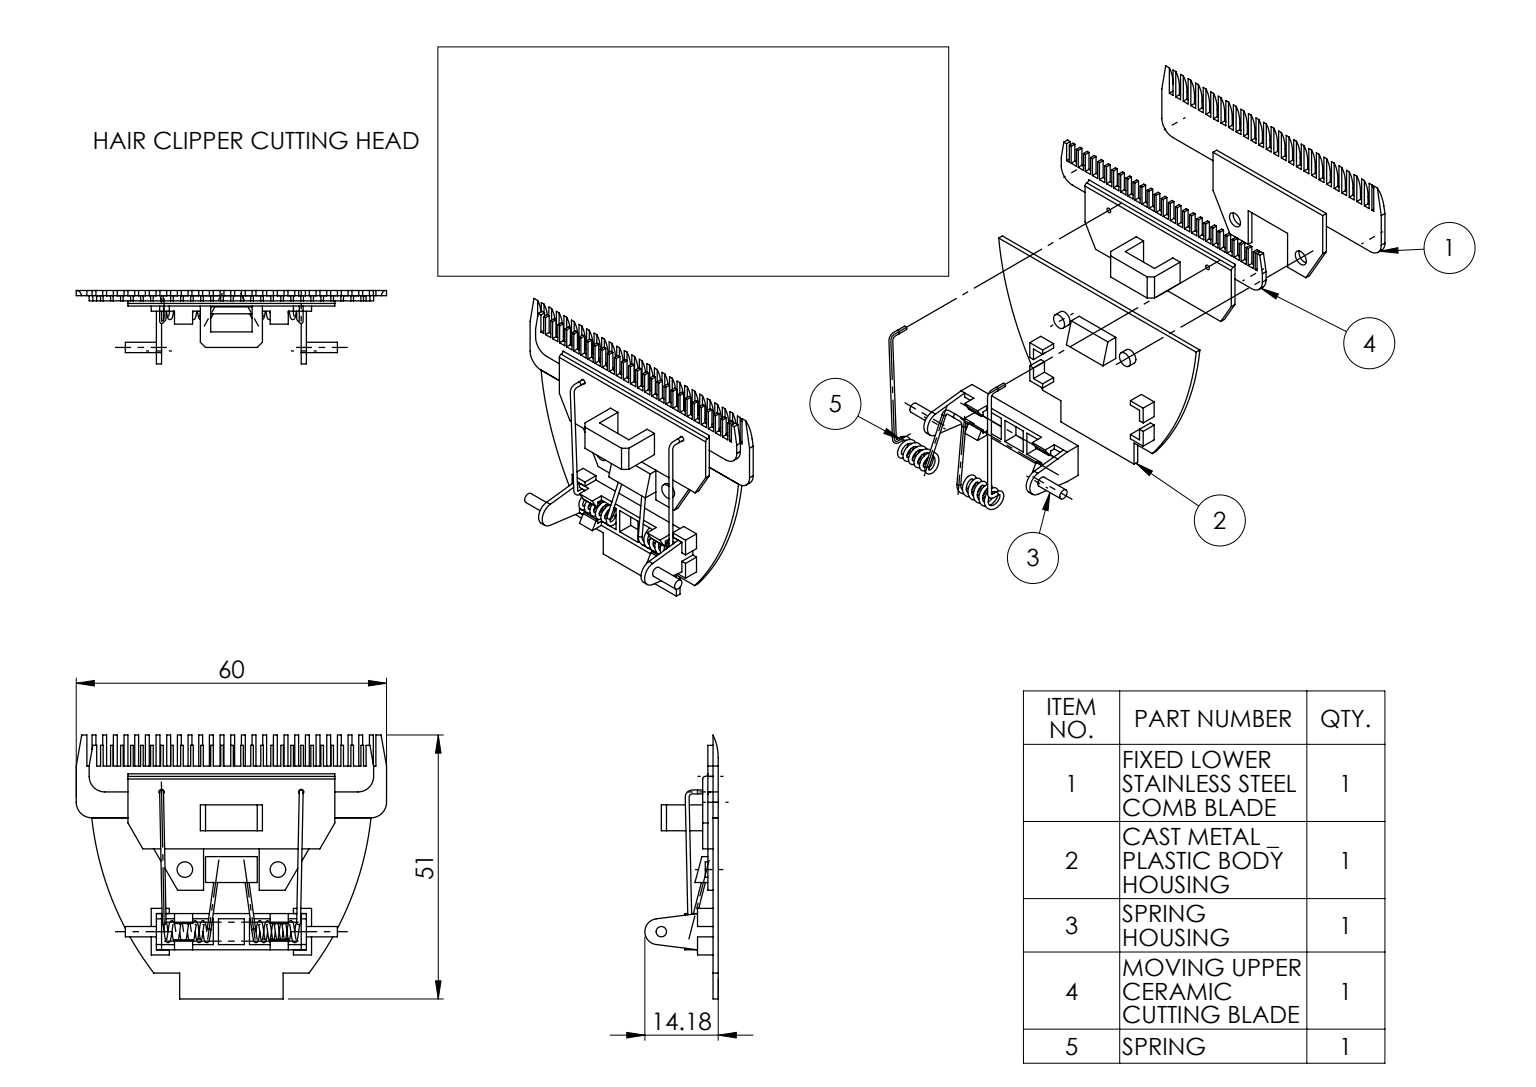
ISO-10303-21;
HEADER;
FILE_DESCRIPTION (('STEP AP214'),
    '1' );
FILE_NAME ('BR-832',
    '2026-10-04T16:38:04',
    ( '' ),
    ( '' ),
    'SwSTEP 2.0',
    'SolidWorks 2026',
    '' );
FILE_SCHEMA (( 'AUTOMOTIVE_DESIGN' ));
ENDSEC;

DATA;
#1 = EDGE_CURVE ( 'NONE', #8973, #13899, #6324, .T. ) ;
#2 = DIRECTION ( 'NONE',  ( -1.000000000000000000, 0.000000000000000000, 0.000000000000000000 ) ) ;
#3 = CARTESIAN_POINT ( 'NONE',  ( -13.45643611822145225, -15.38747602984844853, 4.825999963382285429 ) ) ;
#4 = CARTESIAN_POINT ( 'NONE',  ( 8.871558582316794173, -20.24999999999999289, 3.449312527122348371 ) ) ;
#5 = CARTESIAN_POINT ( 'NONE',  ( -12.62499963760179256, -21.00001830110826972, 4.442557003548452066 ) ) ;
#6 = AXIS2_PLACEMENT_3D ( 'NONE', #19220, #15754, #1437 ) ;
#7 = VECTOR ( 'NONE', #16168, 1000.000000000000000 ) ;
#8 = CARTESIAN_POINT ( 'NONE',  ( -22.81633994409548549, 11.64110105645932691, 0.000000000000000000 ) ) ;
#9 = CARTESIAN_POINT ( 'NONE',  ( -8.309058582316795949, -23.80360840875935935, 1.768074502826626260 ) ) ;
#10 = CARTESIAN_POINT ( 'NONE',  ( 8.496558582316794173, -22.05068747287764452, 1.749999999999998446 ) ) ;
#11 = CARTESIAN_POINT ( 'NONE',  ( 4.097191417683177406, -22.46490103525075810, 4.479004561291653808 ) ) ;
#12 = CARTESIAN_POINT ( 'NONE',  ( -6.621558582316794173, -23.74999999999999645, 3.550687472877651629 ) ) ;
#13 = VERTEX_POINT ( 'NONE', #12698 ) ;
#14 = CARTESIAN_POINT ( 'NONE',  ( 13.82092246150448211, 3.019084305971233562, 5.221833296715730377 ) ) ;
#15 = VECTOR ( 'NONE', #20550, 1000.000000000000000 ) ;
#16 = CARTESIAN_POINT ( 'NONE',  ( -13.49999999999998401, -21.99999999999999645, 11.68378559369222280 ) ) ;
#17 = VERTEX_POINT ( 'NONE', #19101 ) ;
#18 = AXIS2_PLACEMENT_3D ( 'NONE', #8053, #6581, #4805 ) ;
#19 = VERTEX_POINT ( 'NONE', #1418 ) ;
#20 = CARTESIAN_POINT ( 'NONE',  ( 29.44326362367961636, 13.15740888934567288, -2.785412301099487325E-16 ) ) ;
#21 = FACE_BOUND ( 'NONE', #10951, .T. ) ;
#22 = VECTOR ( 'NONE', #3512, 1000.000000000000000 ) ;
#23 = CIRCLE ( 'NONE', #12706, 10.00000000000000000 ) ;
#24 = DIRECTION ( 'NONE',  ( 1.000000000000000000, 0.000000000000000000, 0.000000000000000000 ) ) ;
#25 = CARTESIAN_POINT ( 'NONE',  ( -1.548630333695928396, -9.114917468222230923, 2.372643865078341019 ) ) ;
#26 = FACE_OUTER_BOUND ( 'NONE', #4692, .T. ) ;
#27 = EDGE_CURVE ( 'NONE', #6657, #12771, #12900, .T. ) ;
#28 = CARTESIAN_POINT ( 'NONE',  ( 2.506848361495492394, -9.459347215042898327, 1.711100304737409150 ) ) ;
#29 = CARTESIAN_POINT ( 'NONE',  ( -13.10012427866737639, 3.743776072700027324, 6.001983176248468332 ) ) ;
#30 = CARTESIAN_POINT ( 'NONE',  ( 9.715308582316794173, -23.77099543870833998, 2.825813738724734847 ) ) ;
#31 = CARTESIAN_POINT ( 'NONE',  ( -18.69064177244175795, 11.64110105645932691, 0.000000000000000000 ) ) ;
#32 = CARTESIAN_POINT ( 'NONE',  ( 13.15498530132288479, 5.764257716805535559, 4.666666666666618113 ) ) ;
#33 = CARTESIAN_POINT ( 'NONE',  ( -1.797685059409938280, -9.880079706704160358, 1.626537830816663588 ) ) ;
#34 = ADVANCED_FACE ( 'NONE', ( #11140 ), #17508, .F. ) ;
#35 = ORIENTED_EDGE ( 'NONE', *, *, #2432, .F. ) ;
#36 = ADVANCED_FACE ( 'NONE', ( #7996 ), #7800, .T. ) ;
#37 = CARTESIAN_POINT ( 'NONE',  ( -13.85980676119184629, 4.232741440188380722, 5.965367510457697975 ) ) ;
#38 = CARTESIAN_POINT ( 'NONE',  ( 0.000000000000000000, 10.00000000000000000, 1.000000000000000000 ) ) ;
#39 = CIRCLE ( 'NONE', #18741, 9.999999999999998224 ) ;
#40 = CARTESIAN_POINT ( 'NONE',  ( 5.972191417683178294, -24.47900456129165292, 2.413778621189595963 ) ) ;
#41 = CARTESIAN_POINT ( 'NONE',  ( -6.534691417683177406, -20.97900456129164581, 3.136473910504570917 ) ) ;
#42 = VERTEX_POINT ( 'NONE', #6438 ) ;
#43 = VECTOR ( 'NONE', #1167, 1000.000000000000000 ) ;
#44 = CARTESIAN_POINT ( 'NONE',  ( 13.90439735423812273, 5.734566389025032684, 4.166666666666765551 ) ) ;
#45 = CARTESIAN_POINT ( 'NONE',  ( 13.11017182064853159, 4.251176942750957366, 5.979809059808775196 ) ) ;
#46 = DIRECTION ( 'NONE',  ( 1.000000000000000000, -6.938893903907222067E-15, 0.000000000000000000 ) ) ;
#47 = VECTOR ( 'NONE', #8617, 1000.000000000000000 ) ;
#48 = EDGE_LOOP ( 'NONE', ( #6607, #18673, #6407, #16806 ) ) ;
#49 = VERTEX_POINT ( 'NONE', #11237 ) ;
#50 = PLANE ( 'NONE',  #13438 ) ;
#51 = PLANE ( 'NONE',  #17586 ) ;
#52 = DIRECTION ( 'NONE',  ( 0.000000000000000000, 0.000000000000000000, 1.000000000000000000 ) ) ;
#53 = LINE ( 'NONE', #6129, #8350 ) ;
#54 = AXIS2_PLACEMENT_3D ( 'NONE', #18555, #20450, #10501 ) ;
#55 = EDGE_CURVE ( 'NONE', #14709, #7180, #17615, .T. ) ;
#56 = LINE ( 'NONE', #9565, #7988 ) ;
#57 = CARTESIAN_POINT ( 'NONE',  ( 2.097836924194969033, -11.64739567274323129, 2.830419876579102212 ) ) ;
#58 = LINE ( 'NONE', #8001, #5190 ) ;
#59 = LINE ( 'NONE', #8216, #18452 ) ;
#60 = CARTESIAN_POINT ( 'NONE',  ( 10.05565079891005631, 0.000000000000000000, 1.000000000000000000 ) ) ;
#61 = LINE ( 'NONE', #4966, #6978 ) ;
#62 = DIRECTION ( 'NONE',  ( -5.782411586589356653E-16, 1.000000000000000000, 0.000000000000000000 ) ) ;
#63 = DIRECTION ( 'NONE',  ( 1.000000000000000000, 0.000000000000000000, 0.000000000000000000 ) ) ;
#64 = CARTESIAN_POINT ( 'NONE',  ( 11.77780858231679595, -21.02099543870833998, 3.035098964749253003 ) ) ;
#65 = CARTESIAN_POINT ( 'NONE',  ( -13.08799567112409790, 3.881281391764801025, 5.254907606674271037 ) ) ;
#66 = CARTESIAN_POINT ( 'NONE',  ( -5.309058582316795949, -22.74294823697954016, 2.828734674606448785 ) ) ;
#67 = CARTESIAN_POINT ( 'NONE',  ( -12.25344141768317741, -21.94931252712233061, 1.749999999999998446 ) ) ;
#68 = VERTEX_POINT ( 'NONE', #1726 ) ;
#69 = CARTESIAN_POINT ( 'NONE',  ( 13.09358652029869141, 4.163619275088517035, 5.207983256689002083 ) ) ;
#70 = SURFACE_STYLE_USAGE ( .BOTH. , #17121 ) ;
#71 = ORIENTED_EDGE ( 'NONE', *, *, #17925, .T. ) ;
#72 = ORIENTED_EDGE ( 'NONE', *, *, #11352, .T. ) ;
#73 = AXIS2_PLACEMENT_3D ( 'NONE', #7626, #20402, #7929 ) ;
#74 = DIRECTION ( 'NONE',  ( 1.000000000000000000, 0.000000000000000000, -0.000000000000000000 ) ) ;
#75 = CARTESIAN_POINT ( 'NONE',  ( 13.37505392270939986, -20.99727690317663686, 4.612442573673130930 ) ) ;
#76 = ORIENTED_EDGE ( 'NONE', *, *, #12428, .T. ) ;
#77 = LINE ( 'NONE', #272, #14093 ) ;
#78 = ORIENTED_EDGE ( 'NONE', *, *, #4872, .F. ) ;
#79 = CARTESIAN_POINT ( 'NONE',  ( 10.19094141768317563, -23.27327832286946219, 4.701595411283453707 ) ) ;
#80 = DIRECTION ( 'NONE',  ( -0.000000000000000000, -0.000000000000000000, -1.000000000000000000 ) ) ;
#81 = EDGE_CURVE ( 'NONE', #12312, #20463, #4960, .T. ) ;
#82 = EDGE_CURVE ( 'NONE', #4544, #2802, #3495, .T. ) ;
#83 = CARTESIAN_POINT ( 'NONE',  ( -2.583953725994688533, -9.847075946378776479, 2.560676788604062004 ) ) ;
#84 = CARTESIAN_POINT ( 'NONE',  ( 2.702705060698113115, -10.69015907548275379, 2.777197378435510622 ) ) ;
#85 = CARTESIAN_POINT ( 'NONE',  ( -10.65280858231679240, -21.22443879296942626, 5.229004561291660025 ) ) ;
#86 = VECTOR ( 'NONE', #19310, 1000.000000000000114 ) ;
#87 = LINE ( 'NONE', #11371, #8961 ) ;
#88 = CARTESIAN_POINT ( 'NONE',  ( 5.503441417683177406, -22.05068747287766229, 6.000000000000001776 ) ) ;
#89 =( NAMED_UNIT ( * ) PLANE_ANGLE_UNIT ( ) SI_UNIT ( $, .RADIAN. ) );
#90 = CARTESIAN_POINT ( 'NONE',  ( -3.974842109207561425, -21.82955800590261575, 5.256404853634145447 ) ) ;
#91 = ORIENTED_EDGE ( 'NONE', *, *, #1253, .F. ) ;
#92 = CARTESIAN_POINT ( 'NONE',  ( 13.37155858231679595, -19.49999999999998934, 3.449312527122348371 ) ) ;
#93 = DIRECTION ( 'NONE',  ( -0.000000000000000000, -0.000000000000000000, -1.000000000000000000 ) ) ;
#94 = CARTESIAN_POINT ( 'NONE',  ( -13.90439735423812273, 5.734566389025032684, 4.791666666666684726 ) ) ;
#95 = VERTEX_POINT ( 'NONE', #2332 ) ;
#96 = ADVANCED_FACE ( 'NONE', ( #6747 ), #14788, .T. ) ;
#97 = CARTESIAN_POINT ( 'NONE',  ( 7.465308582316795061, -20.22900456129164937, 4.174186261275266929 ) ) ;
#98 = DIRECTION ( 'NONE',  ( 0.000000000000000000, 1.000000000000000000, 0.000000000000000000 ) ) ;
#99 = ORIENTED_EDGE ( 'NONE', *, *, #2749, .T. ) ;
#100 = DIRECTION ( 'NONE',  ( 0.000000000000000000, 1.000000000000000000, 0.000000000000000000 ) ) ;
#101 = EDGE_LOOP ( 'NONE', ( #4164, #18704, #19121, #9760 ) ) ;
#102 = VECTOR ( 'NONE', #3699, 1000.000000000000000 ) ;
#103 = LINE ( 'NONE', #17562, #12127 ) ;
#104 = ORIENTED_EDGE ( 'NONE', *, *, #13146, .F. ) ;
#105 = CARTESIAN_POINT ( 'NONE',  ( -12.43405858231679595, -23.73192549717337130, 5.303608408759367343 ) ) ;
#106 = CARTESIAN_POINT ( 'NONE',  ( 12.62499979224180180, -20.25001049178813162, 4.458178821399696012 ) ) ;
#107 = DIRECTION ( 'NONE',  ( -1.000000000000000000, 0.000000000000000000, 0.000000000000000000 ) ) ;
#108 = CARTESIAN_POINT ( 'NONE',  ( 0.5631383031621635116, -9.114917468222230923, 1.622643865078341463 ) ) ;
#109 = CARTESIAN_POINT ( 'NONE',  ( 12.62499999999998579, -20.24999999999999289, 3.666666666666653640 ) ) ;
#110 = CARTESIAN_POINT ( 'NONE',  ( -11.00000000000000000, -25.49999999999999645, 6.500000000000000000 ) ) ;
#111 = CARTESIAN_POINT ( 'NONE',  ( -13.37499999999998579, -20.24999999999999289, 3.146526952850934755 ) ) ;
#112 = CARTESIAN_POINT ( 'NONE',  ( 7.840308582316794173, -22.67418626127525982, 5.270995438708342640 ) ) ;
#113 = CARTESIAN_POINT ( 'NONE',  ( -13.89992416064626646, 5.508670112635706495, 5.888743936161951353 ) ) ;
#114 = VECTOR ( 'NONE', #15578, 1000.000000000000000 ) ;
#115 = LINE ( 'NONE', #12457, #8728 ) ;
#116 = CARTESIAN_POINT ( 'NONE',  ( -10.74655858231679595, -21.94931252712234127, 6.000000000000001776 ) ) ;
#117 = CARTESIAN_POINT ( 'NONE',  ( 4.840308582316793284, -22.67418626127525982, 5.270995438708342640 ) ) ;
#118 = EDGE_CURVE ( 'NONE', #8944, #9004, #361, .T. ) ;
#119 = CARTESIAN_POINT ( 'NONE',  ( 8.503441417683177406, -22.05068747287766229, 4.499999999999999112 ) ) ;
#120 = CARTESIAN_POINT ( 'NONE',  ( -9.815941417683177406, -20.79840458871654363, 4.773278322869464851 ) ) ;
#121 = ORIENTED_EDGE ( 'NONE', *, *, #545, .F. ) ;
#122 = VERTEX_POINT ( 'NONE', #13311 ) ;
#123 = CARTESIAN_POINT ( 'NONE',  ( 13.80173896975277437, 2.050317972508536535, 5.200999963382010094 ) ) ;
#124 = CARTESIAN_POINT ( 'NONE',  ( 27.94203811574920948, 16.00000000000000000, 1.000000000000000000 ) ) ;
#125 = CARTESIAN_POINT ( 'NONE',  ( 2.693754455098655409, -10.04853567022903782, 2.237415670251142519 ) ) ;
#126 = ORIENTED_EDGE ( 'NONE', *, *, #7427, .F. ) ;
#127 = EDGE_LOOP ( 'NONE', ( #2197, #15477, #13303, #7881 ) ) ;
#128 = CARTESIAN_POINT ( 'NONE',  ( 5.683390479346035029, 0.000000000000000000, 0.000000000000000000 ) ) ;
#129 = CARTESIAN_POINT ( 'NONE',  ( 0.000000000000000000, 11.64110105645932691, 10.00000000000000000 ) ) ;
#130 = FACE_OUTER_BOUND ( 'NONE', #18306, .T. ) ;
#131 = APPLICATION_CONTEXT ( 'automotive_design' ) ;
#132 = CARTESIAN_POINT ( 'NONE',  ( -2.076833265075072266, -8.407161531158021006, 2.383492984350220389 ) ) ;
#133 = CARTESIAN_POINT ( 'NONE',  ( 0.2815691515810352930, -9.114917468222230923, 2.372643865078523984 ) ) ;
#134 = CARTESIAN_POINT ( 'NONE',  ( -15.11404127825609223, 9.000000000000001776, 0.000000000000000000 ) ) ;
#135 = CARTESIAN_POINT ( 'NONE',  ( -13.09532840572934376, 3.501584489333809724, 5.996774842915142401 ) ) ;
#136 = DIRECTION ( 'NONE',  ( 0.000000000000000000, 0.000000000000000000, -1.000000000000000000 ) ) ;
#137 = LINE ( 'NONE', #12477, #19758 ) ;
#138 = CARTESIAN_POINT ( 'NONE',  ( 13.12175473207386922, 4.086113969730903683, 6.756475741440692850 ) ) ;
#139 = CARTESIAN_POINT ( 'NONE',  ( -1.982945319006538032, -10.83166796549307520, 2.620924705558935308 ) ) ;
#140 = ORIENTED_EDGE ( 'NONE', *, *, #2638, .T. ) ;
#141 = CARTESIAN_POINT ( 'NONE',  ( -13.37499999998404299, -20.99999999996810729, 2.793053905886972998 ) ) ;
#142 = CARTESIAN_POINT ( 'NONE',  ( 6.063547257480584207, 10.00000000000000000, 1.000000000000000000 ) ) ;
#143 = CARTESIAN_POINT ( 'NONE',  ( 5.878441417683177406, -24.50000000000000000, 3.449312527122335048 ) ) ;
#144 = CARTESIAN_POINT ( 'NONE',  ( -6.809058582316796837, -22.74294823697954016, 2.828734674606448785 ) ) ;
#145 = EDGE_LOOP ( 'NONE', ( #572, #13357 ) ) ;
#146 = CARTESIAN_POINT ( 'NONE',  ( 12.62608183053121458, -20.94536755816881168, 4.949360998036265613 ) ) ;
#147 = CARTESIAN_POINT ( 'NONE',  ( 13.10557919622060652, 4.019249409169220577, 6.007898877577752650 ) ) ;
#148 = CARTESIAN_POINT ( 'NONE',  ( -24.79469207716615031, 9.000000000000001776, 1.000000000000000000 ) ) ;
#149 = EDGE_LOOP ( 'NONE', ( #17432, #19814, #17504, #3948 ) ) ;
#150 = EDGE_CURVE ( 'NONE', #20096, #3927, #16331, .T. ) ;
#151 = ORIENTED_EDGE ( 'NONE', *, *, #14900, .F. ) ;
#152 = CARTESIAN_POINT ( 'NONE',  ( -27.94203811574921659, 9.999999999999998224, 1.000000000000000000 ) ) ;
#153 = DIRECTION ( 'NONE',  ( 1.734723475976807094E-15, -1.000000000000000000, 0.000000000000000000 ) ) ;
#154 = EDGE_CURVE ( 'NONE', #3175, #3359, #11545, .T. ) ;
#155 = EDGE_CURVE ( 'NONE', #9432, #10023, #14985, .T. ) ;
#156 = ORIENTED_EDGE ( 'NONE', *, *, #12533, .T. ) ;
#157 = CARTESIAN_POINT ( 'NONE',  ( 0.000000000000000000, 10.00000000000000000, 1.000000000000000000 ) ) ;
#158 = CARTESIAN_POINT ( 'NONE',  ( 0.2815691515810352374, -9.864917468222230923, 1.622643865078524428 ) ) ;
#159 = DIRECTION ( 'NONE',  ( 1.000000000000000000, 0.000000000000000000, 0.000000000000000000 ) ) ;
#160 = CARTESIAN_POINT ( 'NONE',  ( 27.00000000000000000, 3.000000000000000000, 1.000000000000000000 ) ) ;
#161 = CARTESIAN_POINT ( 'NONE',  ( 0.3749999999999968914, 9.000000000000000000, 1.000000000000000000 ) ) ;
#162 = DIRECTION ( 'NONE',  ( -0.000000000000000000, -0.000000000000000000, -1.000000000000000000 ) ) ;
#163 = CARTESIAN_POINT ( 'NONE',  ( -11.12155858231679417, -23.74999999999999645, 3.550687472877651629 ) ) ;
#164 = CARTESIAN_POINT ( 'NONE',  ( -13.09734501894798342, -20.62502179913553846, 3.486720336327766567 ) ) ;
#165 = CARTESIAN_POINT ( 'NONE',  ( -13.08559773465513487, 3.760185600081874746, 5.252303440007609403 ) ) ;
#166 = CARTESIAN_POINT ( 'NONE',  ( -10.84030858231679240, -22.67418626127525982, 5.270995438708342640 ) ) ;
#167 = CARTESIAN_POINT ( 'NONE',  ( -8.784691417683177406, -23.77099543870834353, 4.174186261275252718 ) ) ;
#168 = EDGE_LOOP ( 'NONE', ( #6512, #8849, #9507, #11718, #13942, #16405 ) ) ;
#169 = CARTESIAN_POINT ( 'NONE',  ( 13.37893135632597819, -19.30146650553847465, 4.738802066438188909 ) ) ;
#170 = DIRECTION ( 'NONE',  ( -0.000000000000000000, -0.000000000000000000, -1.000000000000000000 ) ) ;
#171 = ORIENTED_EDGE ( 'NONE', *, *, #6216, .T. ) ;
#172 = ORIENTED_EDGE ( 'NONE', *, *, #1116, .F. ) ;
#173 = DIRECTION ( 'NONE',  ( -0.000000000000000000, -0.000000000000000000, -1.000000000000000000 ) ) ;
#174 = EDGE_CURVE ( 'NONE', #8535, #2052, #465, .T. ) ;
#175 = VERTEX_POINT ( 'NONE', #3806 ) ;
#176 = CARTESIAN_POINT ( 'NONE',  ( -15.00000000000000000, 3.000000000000000000, 1.000000000000000000 ) ) ;
#177 = ORIENTED_EDGE ( 'NONE', *, *, #14375, .F. ) ;
#178 = CARTESIAN_POINT ( 'NONE',  ( 9.628441417683177406, -20.24999999999999289, 3.550687472877664952 ) ) ;
#179 = FACE_OUTER_BOUND ( 'NONE', #19675, .T. ) ;
#180 = AXIS2_PLACEMENT_3D ( 'NONE', #10679, #7642, #12344 ) ;
#181 = CARTESIAN_POINT ( 'NONE',  ( -1.710927537542899612, -9.866086492083725901, 2.372944093759576933 ) ) ;
#182 = CARTESIAN_POINT ( 'NONE',  ( 2.659620708751979645, -10.38426118526329489, 2.698636689302993830 ) ) ;
#183 = CARTESIAN_POINT ( 'NONE',  ( -11.87155858231679417, -20.24999999999999289, 3.449312527122348371 ) ) ;
#184 = EDGE_CURVE ( 'NONE', #2924, #1770, #13210, .T. ) ;
#185 = FILL_AREA_STYLE ('',( #1857 ) ) ;
#186 = CARTESIAN_POINT ( 'NONE',  ( 7.190941417683176518, -23.27327832286946219, 4.701595411283453707 ) ) ;
#187 = LINE ( 'NONE', #10011, #17890 ) ;
#188 = CARTESIAN_POINT ( 'NONE',  ( -6.253441417683176518, -21.94931252712233061, 1.749999999999998446 ) ) ;
#189 = ORIENTED_EDGE ( 'NONE', *, *, #9219, .F. ) ;
#190 = CARTESIAN_POINT ( 'NONE',  ( 11.30905858231679595, -23.80360840875935935, 1.768074502826626260 ) ) ;
#191 = CARTESIAN_POINT ( 'NONE',  ( 12.64387510712649565, -19.29680709011273976, 5.506486987317513737 ) ) ;
#192 = CARTESIAN_POINT ( 'NONE',  ( -12.62562019941893432, -20.21867992933967173, 4.757612834768309540 ) ) ;
#193 = VERTEX_POINT ( 'NONE', #561 ) ;
#194 = FACE_OUTER_BOUND ( 'NONE', #14246, .T. ) ;
#195 = EDGE_CURVE ( 'NONE', #11770, #17871, #16650, .T. ) ;
#196 = LINE ( 'NONE', #13157, #16335 ) ;
#197 = EDGE_CURVE ( 'NONE', #4053, #10774, #19608, .T. ) ;
#198 = EDGE_LOOP ( 'NONE', ( #19605, #1454, #13205, #13918 ) ) ;
#199 = SHAPE_DEFINITION_REPRESENTATION ( #15847, #6045 ) ;
#200 = VERTEX_POINT ( 'NONE', #10184 ) ;
#201 = CARTESIAN_POINT ( 'NONE',  ( -8.376396343307449754, 11.64110105645932691, 0.000000000000000000 ) ) ;
#202 = ORIENTED_EDGE ( 'NONE', *, *, #15005, .F. ) ;
#203 = CARTESIAN_POINT ( 'NONE',  ( -7.277808582316794173, -20.27099543870833642, 2.724438792969431589 ) ) ;
#204 = DIRECTION ( 'NONE',  ( 0.000000000000000000, -1.000000000000000000, 0.000000000000000000 ) ) ;
#205 = DIRECTION ( 'NONE',  ( 0.000000000000000000, -1.000000000000000000, 0.000000000000000000 ) ) ;
#206 = CARTESIAN_POINT ( 'NONE',  ( 2.022757268986824730, -10.07035769906783784, 1.675405020440470238 ) ) ;
#207 = CARTESIAN_POINT ( 'NONE',  ( 12.65410809543883985, -18.78004118034163739, 5.517608176248461227 ) ) ;
#208 = DIRECTION ( 'NONE',  ( -0.9848077530122082424, 0.1736481776669295263, 0.000000000000000000 ) ) ;
#209 = CARTESIAN_POINT ( 'NONE',  ( -13.39169183355864590, -18.65706240528901105, 4.755687463382285429 ) ) ;
#210 = CARTESIAN_POINT ( 'NONE',  ( 8.777808582316797725, -19.52099543870833642, 2.413778621189609286 ) ) ;
#211 = CARTESIAN_POINT ( 'NONE',  ( -12.62500000000001954, -20.24999999999450040, 3.833333333368183382 ) ) ;
#212 = DIRECTION ( 'NONE',  ( -1.000000000000000000, -6.938893903907222067E-15, 0.000000000000000000 ) ) ;
#213 = CARTESIAN_POINT ( 'NONE',  ( 5.215308582316793284, -23.77099543870833998, 2.825813738724734847 ) ) ;
#214 = CARTESIAN_POINT ( 'NONE',  ( 4.565941417683176518, -22.67126532539353789, 2.757051763020445634 ) ) ;
#215 = CARTESIAN_POINT ( 'NONE',  ( -5.409691417683177406, -21.32581373872474373, 5.270995438708348857 ) ) ;
#216 = ORIENTED_EDGE ( 'NONE', *, *, #5288, .T. ) ;
#217 = ORIENTED_EDGE ( 'NONE', *, *, #4935, .T. ) ;
#218 = CARTESIAN_POINT ( 'NONE',  ( 13.82811627091129836, 3.382371681020614584, 5.229645796715683304 ) ) ;
#219 = CYLINDRICAL_SURFACE ( 'NONE', #18842, 10.00000000000000000 ) ;
#220 = ORIENTED_EDGE ( 'NONE', *, *, #415, .T. ) ;
#221 = ORIENTED_EDGE ( 'NONE', *, *, #17663, .T. ) ;
#222 = CARTESIAN_POINT ( 'NONE',  ( -14.56494360078803396, 0.000000000000000000, 0.000000000000000000 ) ) ;
#223 = CYLINDRICAL_SURFACE ( 'NONE', #8699, 10.00000000000000000 ) ;
#224 = CARTESIAN_POINT ( 'NONE',  ( -13.12529397354238192, 5.014845663890295846, 4.833333333333344584 ) ) ;
#225 = CARTESIAN_POINT ( 'NONE',  ( -1.513434189748285918, -8.364917468222230923, 1.622643865078341907 ) ) ;
#226 = CARTESIAN_POINT ( 'NONE',  ( 0.000000000000000000, 11.64110105645932691, 10.00000000000000000 ) ) ;
#227 = EDGE_CURVE ( 'NONE', #2917, #11113, #5373, .T. ) ;
#228 = DIRECTION ( 'NONE',  ( -0.000000000000000000, -0.000000000000000000, -1.000000000000000000 ) ) ;
#229 = CARTESIAN_POINT ( 'NONE',  ( -12.64323021897839006, -19.32937394158751943, 5.504219675487169283 ) ) ;
#230 = DIRECTION ( 'NONE',  ( -1.000000000000000000, -0.000000000000000000, -0.000000000000000000 ) ) ;
#231 = CARTESIAN_POINT ( 'NONE',  ( 3.999999999999999112, -7.500000000000047073, 9.999999999999998224 ) ) ;
#232 = CARTESIAN_POINT ( 'NONE',  ( 12.70700162295422864, -16.85891804079483691, 6.308954579156044851 ) ) ;
#233 = CARTESIAN_POINT ( 'NONE',  ( -2.097836924194969033, -11.64739567274323129, 2.830419876579102212 ) ) ;
#234 = EDGE_LOOP ( 'NONE', ( #6120, #13458, #16622, #14444 ) ) ;
#235 = VECTOR ( 'NONE', #10575, 1000.000000000000000 ) ;
#236 = CARTESIAN_POINT ( 'NONE',  ( -13.70116456325478893, -3.778689555664588973, 5.825679699621801433 ) ) ;
#237 = CARTESIAN_POINT ( 'NONE',  ( 11.99999999999999822, -25.50000000000000355, 4.000000000000000000 ) ) ;
#238 = CARTESIAN_POINT ( 'NONE',  ( 6.534691417683177406, -19.47900456129164581, 2.515153566944927199 ) ) ;
#239 = CARTESIAN_POINT ( 'NONE',  ( -5.027808582316795949, -22.97900456129165647, 3.964901035250747885 ) ) ;
#240 = EDGE_LOOP ( 'NONE', ( #2876, #19889, #3545, #20179 ) ) ;
#241 = CARTESIAN_POINT ( 'NONE',  ( 13.87372783958217681, 4.185755898898970706, 6.732634959205082481 ) ) ;
#242 = CARTESIAN_POINT ( 'NONE',  ( 12.95145221759166354, -3.764163011652346569, 5.840524842913703552 ) ) ;
#243 = CARTESIAN_POINT ( 'NONE',  ( -0.000000000000000000, 10.00000000000000000, 0.000000000000000000 ) ) ;
#244 = ORIENTED_EDGE ( 'NONE', *, *, #20430, .T. ) ;
#245 = ORIENTED_EDGE ( 'NONE', *, *, #7610, .F. ) ;
#246 = LINE ( 'NONE', #152, #17116 ) ;
#247 = LINE ( 'NONE', #19711, #19278 ) ;
#248 = EDGE_LOOP ( 'NONE', ( #4182, #12799, #16047, #1135 ) ) ;
#249 = DIRECTION ( 'NONE',  ( 0.000000000000000000, 0.2487476929738665354, 0.9685683172808094987 ) ) ;
#250 = CARTESIAN_POINT ( 'NONE',  ( 1.337453470010121714, -9.864917468222230923, 1.622643865078341907 ) ) ;
#251 = CARTESIAN_POINT ( 'NONE',  ( -7.500000000000000888, -9.999999999999992895, 1.000000000000000000 ) ) ;
#252 = VECTOR ( 'NONE', #1364, 1000.000000000000000 ) ;
#253 = DIRECTION ( 'NONE',  ( 0.000000000000000000, 0.000000000000000000, -1.000000000000000000 ) ) ;
#254 = EDGE_CURVE ( 'NONE', #12726, #11061, #10084, .T. ) ;
#255 = CARTESIAN_POINT ( 'NONE',  ( -15.49999999999998046, -26.49999999999999645, 4.000000000000000000 ) ) ;
#256 = LINE ( 'NONE', #3402, #19673 ) ;
#257 = CARTESIAN_POINT ( 'NONE',  ( -10.84030858231679240, -22.67418626127525982, 5.270995438708342640 ) ) ;
#258 = CARTESIAN_POINT ( 'NONE',  ( -1.548630333695928396, -9.114917468222230923, 2.372643865078341019 ) ) ;
#259 = EDGE_LOOP ( 'NONE', ( #9919, #6781, #19047, #17582 ) ) ;
#260 = CARTESIAN_POINT ( 'NONE',  ( -12.62837453896009876, -19.32958578251692572, 4.742959489302074338 ) ) ;
#261 = CARTESIAN_POINT ( 'NONE',  ( -6.059058582316795949, -21.25705176302045274, 4.171265325393551215 ) ) ;
#262 = CARTESIAN_POINT ( 'NONE',  ( -4.284691417683176518, -23.77099543870834353, 4.174186261275252718 ) ) ;
#263 = ORIENTED_EDGE ( 'NONE', *, *, #15990, .F. ) ;
#264 = ADVANCED_FACE ( 'NONE', ( #16459 ), #18242, .T. ) ;
#265 = CARTESIAN_POINT ( 'NONE',  ( 13.80173896975277437, 2.050317972508536535, 5.200999963382010094 ) ) ;
#266 = FACE_OUTER_BOUND ( 'NONE', #16647, .T. ) ;
#267 = ORIENTED_EDGE ( 'NONE', *, *, #11944, .F. ) ;
#268 = ORIENTED_EDGE ( 'NONE', *, *, #5212, .F. ) ;
#269 = CARTESIAN_POINT ( 'NONE',  ( -0.000000000000000000, 11.64110105645932691, 0.000000000000000000 ) ) ;
#270 = VECTOR ( 'NONE', #15636, 1000.000000000000000 ) ;
#271 = ORIENTED_EDGE ( 'NONE', *, *, #10983, .T. ) ;
#272 = CARTESIAN_POINT ( 'NONE',  ( 0.000000000000000000, 0.000000000000000000, 0.000000000000000000 ) ) ;
#273 = VECTOR ( 'NONE', #18703, 1000.000000000000000 ) ;
#274 = ORIENTED_EDGE ( 'NONE', *, *, #17333, .T. ) ;
#275 = CARTESIAN_POINT ( 'NONE',  ( 9.815941417683177406, -20.79840458871654363, 4.773278322869464851 ) ) ;
#276 = DIRECTION ( 'NONE',  ( 0.000000000000000000, 0.000000000000000000, 1.000000000000000000 ) ) ;
#277 = CARTESIAN_POINT ( 'NONE',  ( -1.853238653218509890, -9.965882697426144077, 2.398573752920997837 ) ) ;
#278 = LINE ( 'NONE', #14715, #12697 ) ;
#279 = CARTESIAN_POINT ( 'NONE',  ( -9.340308582316794173, -22.67418626127525982, 5.270995438708342640 ) ) ;
#280 = AXIS2_PLACEMENT_3D ( 'NONE', #10758, #15558, #17129 ) ;
#281 = EDGE_CURVE ( 'NONE', #9560, #10619, #19020, .T. ) ;
#282 = AXIS2_PLACEMENT_3D ( 'NONE', #5586, #11856, #17932 ) ;
#283 = FILL_AREA_STYLE ('',( #16193 ) ) ;
#284 = CARTESIAN_POINT ( 'NONE',  ( 10.56594141768317741, -23.20159541128344927, 2.226721677130534705 ) ) ;
#285 = DIRECTION ( 'NONE',  ( 1.000000000000000000, 0.000000000000000000, -0.000000000000000000 ) ) ;
#286 = CARTESIAN_POINT ( 'NONE',  ( -11.59719141768317741, -22.46490103525075810, 4.479004561291653808 ) ) ;
#287 = ORIENTED_EDGE ( 'NONE', *, *, #9934, .F. ) ;
#288 = CARTESIAN_POINT ( 'NONE',  ( 11.68405858231679595, -20.26807450282662160, 1.696391591240633101 ) ) ;
#289 = ADVANCED_FACE ( 'NONE', ( #9873 ), #19713, .T. ) ;
#290 = CARTESIAN_POINT ( 'NONE',  ( 12.64131715375063258, -19.42598373559290792, 5.491151580003103660 ) ) ;
#291 = CARTESIAN_POINT ( 'NONE',  ( -13.15498530132288479, 5.764257716805535559, 4.791666666666684726 ) ) ;
#292 = ORIENTED_EDGE ( 'NONE', *, *, #13482, .F. ) ;
#293 = EDGE_CURVE ( 'NONE', #3359, #13135, #6295, .T. ) ;
#294 = CARTESIAN_POINT ( 'NONE',  ( -3.497260319564023057, 9.000000000000001776, 0.000000000000000000 ) ) ;
#295 = DIRECTION ( 'NONE',  ( 1.000000000000000000, 0.000000000000000000, 0.000000000000000000 ) ) ;
#296 = ORIENTED_EDGE ( 'NONE', *, *, #17959, .F. ) ;
#297 = VECTOR ( 'NONE', #5292, 1000.000000000000000 ) ;
#298 = CIRCLE ( 'NONE', #11982, 10.00000000000000000 ) ;
#299 = PRESENTATION_STYLE_ASSIGNMENT (( #17872 ) ) ;
#300 = ORIENTED_EDGE ( 'NONE', *, *, #6043, .F. ) ;
#301 = EDGE_CURVE ( 'NONE', #14522, #1368, #8723, .T. ) ;
#302 = VECTOR ( 'NONE', #7934, 1000.000000000000000 ) ;
#303 = CARTESIAN_POINT ( 'NONE',  ( 12.87800906051949390, -19.89203723036131066, 3.516308674092069708 ) ) ;
#304 = AXIS2_PLACEMENT_3D ( 'NONE', #2180, #611, #8776 ) ;
#305 = ORIENTED_EDGE ( 'NONE', *, *, #7234, .F. ) ;
#306 = VECTOR ( 'NONE', #18807, 1000.000000000000000 ) ;
#307 = CARTESIAN_POINT ( 'NONE',  ( -6.809058582316794173, -23.27327832286945153, 2.298404588716537411 ) ) ;
#308 = CARTESIAN_POINT ( 'NONE',  ( 13.12463908936614132, 4.981774012991869505, 5.264611377988129171 ) ) ;
#309 = CARTESIAN_POINT ( 'NONE',  ( 18.44064177244175440, 16.00000000000000000, 1.000000000000000000 ) ) ;
#310 = EDGE_CURVE ( 'NONE', #175, #19704, #17077, .T. ) ;
#311 = CARTESIAN_POINT ( 'NONE',  ( 12.62499999999998401, -20.24999999999998934, 2.439580858552613751 ) ) ;
#312 = PLANE ( 'NONE',  #2667 ) ;
#313 = CARTESIAN_POINT ( 'NONE',  ( -13.53317008522746434, -11.51241069598931510, 4.909333296715523431 ) ) ;
#314 = CIRCLE ( 'NONE', #14674, 10.00000000000000000 ) ;
#315 = AXIS2_PLACEMENT_3D ( 'NONE', #4243, #16683, #17105 ) ;
#316 = CARTESIAN_POINT ( 'NONE',  ( 7.559058582316795949, -20.19639159124062999, 5.231925497173373074 ) ) ;
#317 = CARTESIAN_POINT ( 'NONE',  ( -13.15498530132288479, 5.764257716805535559, 3.666666666666500873 ) ) ;
#318 = CARTESIAN_POINT ( 'NONE',  ( -10.00344141768317741, -22.05068747287766229, 6.000000000000001776 ) ) ;
#319 = VECTOR ( 'NONE', #10177, 1000.000000000000000 ) ;
#320 = DIRECTION ( 'NONE',  ( 0.000000000000000000, -0.000000000000000000, 1.000000000000000000 ) ) ;
#321 = CARTESIAN_POINT ( 'NONE',  ( -7.500000000000000000, -20.16506350946107418, 5.000000000000000000 ) ) ;
#322 = CARTESIAN_POINT ( 'NONE',  ( 10.93405858231679595, -22.67126532539354855, 4.242948236979545484 ) ) ;
#323 = CARTESIAN_POINT ( 'NONE',  ( -6.722191417683176518, -20.27099543870833998, 4.275561207030583510 ) ) ;
#324 = ORIENTED_EDGE ( 'NONE', *, *, #17670, .T. ) ;
#325 = ORIENTED_EDGE ( 'NONE', *, *, #12049, .T. ) ;
#326 = CARTESIAN_POINT ( 'NONE',  ( 13.37883250981221472, -20.05645825448334563, 5.102688967256983510 ) ) ;
#327 = DIRECTION ( 'NONE',  ( 0.000000000000000000, 0.000000000000000000, -1.000000000000000000 ) ) ;
#328 = CARTESIAN_POINT ( 'NONE',  ( 9.830951894845298966, -7.500000000000047073, 7.000000000000000000 ) ) ;
#329 = ORIENTED_EDGE ( 'NONE', *, *, #3787, .F. ) ;
#330 = EDGE_CURVE ( 'NONE', #20408, #13997, #13927, .T. ) ;
#331 = EDGE_LOOP ( 'NONE', ( #16127, #14470, #13660, #8482 ) ) ;
#332 = CARTESIAN_POINT ( 'NONE',  ( -7.500000000000000000, -20.16506350946107418, 5.250000000000000000 ) ) ;
#333 = CARTESIAN_POINT ( 'NONE',  ( -2.187849085826861550, 10.00000000000000000, 0.000000000000000000 ) ) ;
#334 = CARTESIAN_POINT ( 'NONE',  ( 13.66279757975024722, -5.716222222589476765, 5.784013032957989964 ) ) ;
#335 = VECTOR ( 'NONE', #866, 1000.000000000000000 ) ;
#336 = CARTESIAN_POINT ( 'NONE',  ( 4.750698171653723989, 10.00000000000000000, 1.000000000000000000 ) ) ;
#337 = VECTOR ( 'NONE', #729, 1000.000000000000000 ) ;
#338 = EDGE_CURVE ( 'NONE', #6318, #18399, #16985, .T. ) ;
#339 = EDGE_CURVE ( 'NONE', #9554, #1664, #7256, .T. ) ;
#340 = CARTESIAN_POINT ( 'NONE',  ( 0.000000000000000000, 4.999999999999999112, 1.000000000000000000 ) ) ;
#341 = CARTESIAN_POINT ( 'NONE',  ( -13.10756170493883310, 4.119366099410778581, 6.001761809183453700 ) ) ;
#342 = CARTESIAN_POINT ( 'NONE',  ( 5.309058582316794173, -23.27327832286945153, 2.298404588716537411 ) ) ;
#343 = PLANE ( 'NONE',  #7411 ) ;
#344 = CARTESIAN_POINT ( 'NONE',  ( 12.65650603190776025, -18.65894538865861563, 5.520212342915047365 ) ) ;
#345 = CARTESIAN_POINT ( 'NONE',  ( -0.2815691515810352374, -9.864917468222230923, 2.372643865078523540 ) ) ;
#346 = VERTEX_POINT ( 'NONE', #16765 ) ;
#347 = CARTESIAN_POINT ( 'NONE',  ( -13.39902456816392906, -19.03675930772010361, 5.497554699623231400 ) ) ;
#348 = CARTESIAN_POINT ( 'NONE',  ( -1.734723475976795735E-14, 10.00000000000004619, 1.000000000000000000 ) ) ;
#349 = CARTESIAN_POINT ( 'NONE',  ( 10.09719141768317741, -22.77556120703057729, 5.229004561291655584 ) ) ;
#350 = CARTESIAN_POINT ( 'NONE',  ( -7.371558582316795949, -20.99999999999999645, 3.449312527122348371 ) ) ;
#351 = VERTEX_POINT ( 'NONE', #5579 ) ;
#352 = CARTESIAN_POINT ( 'NONE',  ( 13.87486364728600208, 4.243114187942282456, 6.725269602253773016 ) ) ;
#353 = CARTESIAN_POINT ( 'NONE',  ( 12.66849571425264287, -18.05346643024382303, 5.533233176248494978 ) ) ;
#354 = CARTESIAN_POINT ( 'NONE',  ( -7.499999999999999112, -18.49999999999999645, 4.000000000000000000 ) ) ;
#355 = ORIENTED_EDGE ( 'NONE', *, *, #1510, .F. ) ;
#356 = EDGE_CURVE ( 'NONE', #19341, #13538, #2755, .T. ) ;
#357 = VECTOR ( 'NONE', #14447, 1000.000000000000000 ) ;
#358 = ORIENTED_EDGE ( 'NONE', *, *, #6960, .T. ) ;
#359 = DIRECTION ( 'NONE',  ( -5.782411586589356653E-16, 1.000000000000000000, 0.000000000000000000 ) ) ;
#360 = CARTESIAN_POINT ( 'NONE',  ( 1.811130159782011528, 4.999999999999999112, 0.000000000000000000 ) ) ;
#361 = LINE ( 'NONE', #7053, #18342 ) ;
#362 = VECTOR ( 'NONE', #20394, 1000.000000000000000 ) ;
#363 = CARTESIAN_POINT ( 'NONE',  ( 0.000000000000000000, 10.00000000000000000, 1.000000000000000000 ) ) ;
#364 = CARTESIAN_POINT ( 'NONE',  ( 1.711347482507859397, -9.865394108634699677, 1.622766275858107621 ) ) ;
#365 = CARTESIAN_POINT ( 'NONE',  ( 7.499999999999999112, -23.83493649053891517, 5.249999999999999112 ) ) ;
#366 = CARTESIAN_POINT ( 'NONE',  ( 26.04469207716615031, 4.999999999999999112, 0.000000000000000000 ) ) ;
#367 = VECTOR ( 'NONE', #7889, 1000.000000000000000 ) ;
#368 = VECTOR ( 'NONE', #17912, 1000.000000000000000 ) ;
#369 = DIRECTION ( 'NONE',  ( -0.000000000000000000, 0.000000000000000000, -1.000000000000000000 ) ) ;
#370 = DIRECTION ( 'NONE',  ( 0.000000000000000000, 1.000000000000000000, 0.000000000000000000 ) ) ;
#371 = CARTESIAN_POINT ( 'NONE',  ( -9.059058582316794173, -20.72672167713054137, 4.701595411283463477 ) ) ;
#372 = VECTOR ( 'NONE', #20232, 1000.000000000000000 ) ;
#373 = CARTESIAN_POINT ( 'NONE',  ( -0.5631383031621635116, -9.114917468222230923, 2.372643865078341019 ) ) ;
#374 = EDGE_LOOP ( 'NONE', ( #263, #11336, #20204, #3234 ) ) ;
#375 = CARTESIAN_POINT ( 'NONE',  ( -12.62499994688180749, -19.50000268246798640, 4.473800639250938183 ) ) ;
#376 = CARTESIAN_POINT ( 'NONE',  ( -10.37155858231679417, -20.24999999999999289, 3.449312527122348371 ) ) ;
#377 = CARTESIAN_POINT ( 'NONE',  ( -7.284691417683176518, -23.77099543870834353, 4.174186261275252718 ) ) ;
#378 = VERTEX_POINT ( 'NONE', #17178 ) ;
#379 = CARTESIAN_POINT ( 'NONE',  ( 13.37930517931174634, -19.28258844475809042, 4.742233558278135419 ) ) ;
#380 = CARTESIAN_POINT ( 'NONE',  ( -7.500000000000000000, -18.49999999999999645, 6.500000000000000888 ) ) ;
#381 = VERTEX_POINT ( 'NONE', #2855 ) ;
#382 = VERTEX_POINT ( 'NONE', #11949 ) ;
#383 = ADVANCED_FACE ( 'NONE', ( #12259 ), #18550, .T. ) ;
#384 = LINE ( 'NONE', #6768, #18444 ) ;
#385 = ORIENTED_EDGE ( 'NONE', *, *, #8922, .T. ) ;
#386 = CARTESIAN_POINT ( 'NONE',  ( -14.99999999999998046, -26.49999999999999645, 4.000000000000000000 ) ) ;
#387 = VECTOR ( 'NONE', #11320, 1000.000000000000000 ) ;
#388 = ORIENTED_EDGE ( 'NONE', *, *, #15625, .T. ) ;
#389 = CARTESIAN_POINT ( 'NONE',  ( 6.909691417683177406, -21.32581373872474373, 5.270995438708348857 ) ) ;
#390 = DIRECTION ( 'NONE',  ( 0.000000000000000000, 1.000000000000000000, 0.000000000000000000 ) ) ;
#391 = CARTESIAN_POINT ( 'NONE',  ( -1.707060460004204527, -9.864918773552613374, 2.372644200313257290 ) ) ;
#392 = DIRECTION ( 'NONE',  ( 0.000000000000000000, 0.000000000000000000, 1.000000000000000000 ) ) ;
#393 = CARTESIAN_POINT ( 'NONE',  ( -7.840308582316794173, -22.67418626127525982, 5.270995438708342640 ) ) ;
#394 = PRESENTATION_STYLE_ASSIGNMENT (( #14290 ) ) ;
#395 = CARTESIAN_POINT ( 'NONE',  ( 8.690941417683177406, -23.27327832286946219, 4.701595411283453707 ) ) ;
#396 = LINE ( 'NONE', #10120, #18568 ) ;
#397 = CARTESIAN_POINT ( 'NONE',  ( -10.47219141768317741, -22.97900456129165292, 3.035098964749240125 ) ) ;
#398 = AXIS2_PLACEMENT_3D ( 'NONE', #19475, #19368, #6705 ) ;
#399 = ORIENTED_EDGE ( 'NONE', *, *, #570, .F. ) ;
#400 = CARTESIAN_POINT ( 'NONE',  ( 9.621558582316795949, -24.50000000000000000, 3.550687472877651629 ) ) ;
#401 = CARTESIAN_POINT ( 'NONE',  ( 13.09532840572934376, 3.501584489333809724, 5.996774842915142401 ) ) ;
#402 = CARTESIAN_POINT ( 'NONE',  ( -13.15498530132288479, 5.764257716805535559, 4.333333333333380999 ) ) ;
#403 = ORIENTED_EDGE ( 'NONE', *, *, #20429, .T. ) ;
#404 = DIRECTION ( 'NONE',  ( 1.000000000000000000, 0.000000000000000000, -0.000000000000000000 ) ) ;
#405 = CARTESIAN_POINT ( 'NONE',  ( 26.69203811574920238, 11.64110105645932691, 0.000000000000000000 ) ) ;
#406 = ORIENTED_EDGE ( 'NONE', *, *, #5858, .F. ) ;
#407 = APPLICATION_PROTOCOL_DEFINITION ( 'draft international standard', 'automotive_design', 1998, #17226 ) ;
#408 = ORIENTED_EDGE ( 'NONE', *, *, #19426, .T. ) ;
#409 = EDGE_CURVE ( 'NONE', #6506, #12491, #9133, .T. ) ;
#410 = CARTESIAN_POINT ( 'NONE',  ( 13.24164500767265729, -19.96139048183125198, 3.467035629977988975 ) ) ;
#411 = VERTEX_POINT ( 'NONE', #5686 ) ;
#412 = CARTESIAN_POINT ( 'NONE',  ( -27.94203811574921303, 11.64110105645932691, 10.00000000000000000 ) ) ;
#413 = VECTOR ( 'NONE', #1830, 1000.000000000000000 ) ;
#414 = CARTESIAN_POINT ( 'NONE',  ( 13.05696142222617695, 1.564051822406025583, 5.955108176248398166 ) ) ;
#415 = EDGE_CURVE ( 'NONE', #11125, #7180, #2437, .T. ) ;
#416 = DIRECTION ( 'NONE',  ( 0.000000000000000000, 1.000000000000000000, 0.000000000000000000 ) ) ;
#417 = EDGE_CURVE ( 'NONE', #11328, #740, #20025, .T. ) ;
#418 = CARTESIAN_POINT ( 'NONE',  ( 13.15498501280115917, 5.764243146453090105, 5.045733045595949484 ) ) ;
#419 = CARTESIAN_POINT ( 'NONE',  ( 4.315753587183824180, -21.65797192216093947, 4.831781436261117335 ) ) ;
#420 = CARTESIAN_POINT ( 'NONE',  ( -13.37499979530394967, -20.25001033714808329, 4.458488164327452097 ) ) ;
#421 = CARTESIAN_POINT ( 'NONE',  ( 9.715308582316795949, -24.52099543870834708, 2.515153566944913432 ) ) ;
#422 = AXIS2_PLACEMENT_3D ( 'NONE', #14755, #433, #5548 ) ;
#423 = CARTESIAN_POINT ( 'NONE',  ( -13.14123030749026277, 5.069630528265579805, 6.418963484850015000 ) ) ;
#424 = CARTESIAN_POINT ( 'NONE',  ( -12.44094141768317741, -20.19639159124061933, 1.768074502826635586 ) ) ;
#425 = FACE_OUTER_BOUND ( 'NONE', #12281, .T. ) ;
#426 = CARTESIAN_POINT ( 'NONE',  ( 3.944195004867014909, -21.61378581760806128, 5.207602947182413011 ) ) ;
#427 = VECTOR ( 'NONE', #3877, 1000.000000000000000 ) ;
#428 = CARTESIAN_POINT ( 'NONE',  ( 10.84030858231679595, -22.36352608949544418, 4.520995438708343528 ) ) ;
#429 = CARTESIAN_POINT ( 'NONE',  ( -7.284691417683176518, -23.77099543870834353, 4.174186261275251830 ) ) ;
#430 = ORIENTED_EDGE ( 'NONE', *, *, #12679, .F. ) ;
#431 = VERTEX_POINT ( 'NONE', #15503 ) ;
#432 = CARTESIAN_POINT ( 'NONE',  ( 13.84501469867711698, 4.235742283194553259, 4.791666666666684726 ) ) ;
#433 = DIRECTION ( 'NONE',  ( 0.000000000000000000, -0.5000000000000041078, -0.8660254037844363761 ) ) ;
#434 = DIRECTION ( 'NONE',  ( -0.000000000000000000, -0.000000000000000000, -1.000000000000000000 ) ) ;
#435 = ORIENTED_EDGE ( 'NONE', *, *, #9741, .F. ) ;
#436 = ADVANCED_FACE ( 'NONE', ( #18652 ), #4141, .F. ) ;
#437 = DIRECTION ( 'NONE',  ( 1.000000000000000000, 5.204170427930411817E-15, -0.000000000000000000 ) ) ;
#438 = DIRECTION ( 'NONE',  ( -1.000000000000000000, -0.000000000000000000, -0.000000000000000000 ) ) ;
#439 = CARTESIAN_POINT ( 'NONE',  ( 13.84983662433050178, 3.729249528687784920, 5.987138032956566214 ) ) ;
#440 = DIRECTION ( 'NONE',  ( 1.000000000000000000, 0.000000000000000000, 0.000000000000000000 ) ) ;
#441 = CARTESIAN_POINT ( 'NONE',  ( 3.767139617958116471, -12.99583330722436791, 3.561955564372631500 ) ) ;
#442 = VECTOR ( 'NONE', #9719, 1000.000000000000000 ) ;
#443 = CARTESIAN_POINT ( 'NONE',  ( 11.00000000000000000, -25.49999999999999645, 6.500000000000000000 ) ) ;
#444 = CARTESIAN_POINT ( 'NONE',  ( -12.62746768552656285, -19.37538188090202596, 4.723115281690125400 ) ) ;
#445 = CARTESIAN_POINT ( 'NONE',  ( 8.496558582316794173, -22.05068747287764452, 1.749999999999998446 ) ) ;
#446 = CYLINDRICAL_SURFACE ( 'NONE', #17752, 10.00000000000000000 ) ;
#447 = CARTESIAN_POINT ( 'NONE',  ( 13.08573665985359824, 3.017201322601628100, 5.986358176248492313 ) ) ;
#448 = EDGE_CURVE ( 'NONE', #18810, #17042, #19331, .T. ) ;
#449 = CARTESIAN_POINT ( 'NONE',  ( -2.875042468481914248, -11.91375063635796039, 3.091440134965714126 ) ) ;
#450 = CARTESIAN_POINT ( 'NONE',  ( 10.55905858231679595, -21.25705176302045274, 4.171265325393551215 ) ) ;
#451 = CARTESIAN_POINT ( 'NONE',  ( 9.628441417683177406, -20.24999999999999289, 3.550687472877664952 ) ) ;
#452 = VECTOR ( 'NONE', #1980, 1000.000000000000000 ) ;
#453 = CARTESIAN_POINT ( 'NONE',  ( -7.090308582316795061, -21.63647391050454871, 2.479004561291657804 ) ) ;
#454 = ORIENTED_EDGE ( 'NONE', *, *, #14597, .T. ) ;
#455 = CARTESIAN_POINT ( 'NONE',  ( 13.88045627189955233, 4.525541730927888473, 6.662882075361062029 ) ) ;
#456 = CARTESIAN_POINT ( 'NONE',  ( 13.10372118337080849, 3.925419760224517329, 6.005889426248455010 ) ) ;
#457 = CARTESIAN_POINT ( 'NONE',  ( -17.05017143803810242, 9.000000000000001776, 0.000000000000000000 ) ) ;
#458 = VERTEX_POINT ( 'NONE', #10427 ) ;
#459 = ADVANCED_FACE ( 'NONE', ( #3832 ), #17953, .T. ) ;
#460 = EDGE_LOOP ( 'NONE', ( #13036, #3328, #19557, #13078 ) ) ;
#461 = ADVANCED_FACE ( 'NONE', ( #3622 ), #6973, .T. ) ;
#462 = DIRECTION ( 'NONE',  ( 1.000000000000000000, 0.000000000000000000, -0.000000000000000000 ) ) ;
#463 = DIRECTION ( 'NONE',  ( 0.000000000000000000, 1.000000000000000000, -0.000000000000000000 ) ) ;
#464 = AXIS2_PLACEMENT_3D ( 'NONE', #5893, #7568, #2859 ) ;
#465 = LINE ( 'NONE', #16554, #12981 ) ;
#466 = DIRECTION ( 'NONE',  ( -0.000000000000000000, -0.000000000000000000, -1.000000000000000000 ) ) ;
#467 = VECTOR ( 'NONE', #4908, 1000.000000000000000 ) ;
#468 = CARTESIAN_POINT ( 'NONE',  ( 0.000000000000000000, -9.114917468222230923, 1.622643865078341019 ) ) ;
#469 = LINE ( 'NONE', #14791, #1048 ) ;
#470 = DIRECTION ( 'NONE',  ( 1.000000000000000000, 0.000000000000000000, 0.000000000000000000 ) ) ;
#471 = EDGE_CURVE ( 'NONE', #20320, #1300, #20347, .T. ) ;
#472 = CARTESIAN_POINT ( 'NONE',  ( 13.36732475835166234, -20.34061592879088920, 3.450098321863545703 ) ) ;
#473 = CARTESIAN_POINT ( 'NONE',  ( -2.436080212393455735, -9.483920418190111334, 2.467411194204634839 ) ) ;
#474 = CARTESIAN_POINT ( 'NONE',  ( -8.871558582316794173, -20.24999999999999289, 3.449312527122348371 ) ) ;
#475 = CARTESIAN_POINT ( 'NONE',  ( -3.034277558025862298, -9.029550313327863620, 2.543334857076493094 ) ) ;
#476 = ORIENTED_EDGE ( 'NONE', *, *, #6440, .F. ) ;
#477 = CARTESIAN_POINT ( 'NONE',  ( -12.62506359033936754, -19.49678868786235597, 4.541393094775662220 ) ) ;
#478 = CARTESIAN_POINT ( 'NONE',  ( -5.871558582316794173, -20.24999999999999289, 3.449312527122348371 ) ) ;
#479 = CARTESIAN_POINT ( 'NONE',  ( -5.972191417683179182, -23.72900456129165292, 2.724438792969417822 ) ) ;
#480 = ORIENTED_EDGE ( 'NONE', *, *, #12324, .T. ) ;
#481 = CARTESIAN_POINT ( 'NONE',  ( 13.84485691484488257, 4.227774199669918964, 5.063753864839139140 ) ) ;
#482 = ORIENTED_EDGE ( 'NONE', *, *, #7824, .T. ) ;
#483 = VERTEX_POINT ( 'NONE', #11877 ) ;
#484 = CARTESIAN_POINT ( 'NONE',  ( 0.000000000000000000, 9.000000000000001776, 1.000000000000000000 ) ) ;
#485 = VERTEX_POINT ( 'NONE', #18066 ) ;
#486 = CARTESIAN_POINT ( 'NONE',  ( 15.00000000000001776, -26.49999999999999645, 1.000000000000000000 ) ) ;
#487 = VERTEX_POINT ( 'NONE', #8855 ) ;
#488 = CARTESIAN_POINT ( 'NONE',  ( 5.690941417683176518, -23.27327832286946219, 4.701595411283453707 ) ) ;
#489 = DIRECTION ( 'NONE',  ( 0.000000000000000000, -1.000000000000000000, 0.000000000000000000 ) ) ;
#490 = LINE ( 'NONE', #6775, #4650 ) ;
#491 = PLANE ( 'NONE',  #4290 ) ;
#492 = EDGE_CURVE ( 'NONE', #1847, #19275, #12685, .T. ) ;
#493 = CARTESIAN_POINT ( 'NONE',  ( 3.999999999999999112, -2.500000000000047518, 7.000000000000000000 ) ) ;
#494 = CARTESIAN_POINT ( 'NONE',  ( 11.03469141768318273, -20.22900456129164581, 2.825813738724747726 ) ) ;
#495 = CARTESIAN_POINT ( 'NONE',  ( -11.24178095869206828, 0.000000000000000000, 1.000000000000000000 ) ) ;
#496 = CARTESIAN_POINT ( 'NONE',  ( -8.878441417683177406, -22.99999999999999645, 3.449312527122335048 ) ) ;
#497 = CARTESIAN_POINT ( 'NONE',  ( -8.965308582316795949, -19.47900456129164937, 4.484846433055089676 ) ) ;
#498 = ORIENTED_EDGE ( 'NONE', *, *, #11572, .F. ) ;
#499 = CARTESIAN_POINT ( 'NONE',  ( 12.62499999998404121, -20.24999999996810729, 2.793053905886972998 ) ) ;
#500 = CARTESIAN_POINT ( 'NONE',  ( -13.15469878640066526, 5.749788713235649773, 5.232478742873432509 ) ) ;
#501 = ORIENTED_EDGE ( 'NONE', *, *, #15488, .T. ) ;
#502 = DIRECTION ( 'NONE',  ( -0.000000000000000000, -0.000000000000000000, -1.000000000000000000 ) ) ;
#503 = CARTESIAN_POINT ( 'NONE',  ( 30.00000000000000000, 3.000000000000000000, 0.000000000000000000 ) ) ;
#504 = ORIENTED_EDGE ( 'NONE', *, *, #11433, .F. ) ;
#505 =( NAMED_UNIT ( * ) PLANE_ANGLE_UNIT ( ) SI_UNIT ( $, .RADIAN. ) );
#506 = ORIENTED_EDGE ( 'NONE', *, *, #871, .T. ) ;
#507 = CARTESIAN_POINT ( 'NONE',  ( 2.592143777221601386, -9.905122062175031772, 2.575584190728205325 ) ) ;
#508 = VECTOR ( 'NONE', #11618, 1000.000000000000000 ) ;
#509 =( GEOMETRIC_REPRESENTATION_CONTEXT ( 3 ) GLOBAL_UNCERTAINTY_ASSIGNED_CONTEXT ( ( #11112 ) ) GLOBAL_UNIT_ASSIGNED_CONTEXT ( ( #4790, #89, #18824 ) ) REPRESENTATION_CONTEXT ( 'NONE', 'WORKASPACE' ) );
#510 = VERTEX_POINT ( 'NONE', #18268 ) ;
#511 = DIRECTION ( 'NONE',  ( 0.000000000000000000, 1.000000000000000000, -0.000000000000000000 ) ) ;
#512 = CARTESIAN_POINT ( 'NONE',  ( 13.12529380813666435, 5.014837310896125722, 5.033295791462342628 ) ) ;
#513 = CARTESIAN_POINT ( 'NONE',  ( -0.000000000000000000, 11.64110105645932691, 0.000000000000000000 ) ) ;
#514 = VECTOR ( 'NONE', #18897, 1000.000000000000000 ) ;
#515 = CARTESIAN_POINT ( 'NONE',  ( 12.91308523408712183, -5.701695678577235249, 5.798858176249892082 ) ) ;
#516 = CARTESIAN_POINT ( 'NONE',  ( -13.50000000000000178, 0.000000000000000000, 2.000000000000000000 ) ) ;
#517 = CARTESIAN_POINT ( 'NONE',  ( 7.184058582316795949, -20.26807450282662160, 1.696391591240633101 ) ) ;
#518 = CARTESIAN_POINT ( 'NONE',  ( -13.15498530132288479, 5.764257716805535559, 4.166666666666765551 ) ) ;
#519 = CARTESIAN_POINT ( 'NONE',  ( -4.687312169500634340, -21.32903648725300272, 5.908812401261035241 ) ) ;
#520 = EDGE_CURVE ( 'NONE', #9432, #6659, #2464, .T. ) ;
#521 = DIRECTION ( 'NONE',  ( 1.000000000000000000, 0.000000000000000000, 0.000000000000000000 ) ) ;
#522 = PLANE ( 'NONE',  #398 ) ;
#523 = VECTOR ( 'NONE', #704, 1000.000000000000000 ) ;
#524 = CARTESIAN_POINT ( 'NONE',  ( 8.309058582316795949, -22.74294823697954016, 2.828734674606448785 ) ) ;
#525 = DIRECTION ( 'NONE',  ( 0.000000000000000000, 0.000000000000000000, -1.000000000000000000 ) ) ;
#526 = ORIENTED_EDGE ( 'NONE', *, *, #18607, .T. ) ;
#527 = ORIENTED_EDGE ( 'NONE', *, *, #9483, .F. ) ;
#528 = EDGE_CURVE ( 'NONE', #5816, #15348, #13237, .T. ) ;
#529 = CARTESIAN_POINT ( 'NONE',  ( 13.39542766346049518, -19.21840299524461315, 5.493648449623241170 ) ) ;
#530 = ADVANCED_FACE ( 'NONE', ( #697 ), #13548, .T. ) ;
#531 = FACE_OUTER_BOUND ( 'NONE', #8969, .T. ) ;
#532 = ORIENTED_EDGE ( 'NONE', *, *, #6304, .F. ) ;
#533 = DIRECTION ( 'NONE',  ( 0.000000000000000000, 0.000000000000000000, 1.000000000000000000 ) ) ;
#534 = LINE ( 'NONE', #6912, #4355 ) ;
#535 = FACE_OUTER_BOUND ( 'NONE', #13184, .T. ) ;
#536 = CARTESIAN_POINT ( 'NONE',  ( 13.83544900551672185, 3.002674778589386140, 5.971513032956590195 ) ) ;
#537 = SHAPE_REPRESENTATION ( 'Moving Upper Ceramic Cutting Blade', ( #18039 ), #19052 ) ;
#538 = DIRECTION ( 'NONE',  ( -0.000000000000000000, -0.000000000000000000, -1.000000000000000000 ) ) ;
#539 = CARTESIAN_POINT ( 'NONE',  ( 1.797604806073912709, -9.120796646272857799, 2.374153755450133740 ) ) ;
#540 = CARTESIAN_POINT ( 'NONE',  ( 1.652577328807104839, -9.114908150887895744, 1.622641472200749835 ) ) ;
#541 = CARTESIAN_POINT ( 'NONE',  ( -12.93692567357942202, -3.747753484270499591, 5.090845106672844622 ) ) ;
#542 = CARTESIAN_POINT ( 'NONE',  ( 7.840308582316794173, -22.67418626127525982, 5.270995438708342640 ) ) ;
#543 = CARTESIAN_POINT ( 'NONE',  ( -26.79469207716615387, 9.000000000000001776, 0.000000000000000000 ) ) ;
#544 = CARTESIAN_POINT ( 'NONE',  ( 13.11514659413808737, 4.502403003978772134, 5.887634658581065494 ) ) ;
#545 = EDGE_CURVE ( 'NONE', #15372, #1213, #2256, .T. ) ;
#546 = CARTESIAN_POINT ( 'NONE',  ( -1.548630333695928396, -9.114917468222230923, 2.372643865078341019 ) ) ;
#547 = CARTESIAN_POINT ( 'NONE',  ( 6.902808582316795949, -22.46490103525074034, 2.520995438708341307 ) ) ;
#548 = VECTOR ( 'NONE', #15264, 1000.000000000000000 ) ;
#549 = CARTESIAN_POINT ( 'NONE',  ( 8.128441417683175629, -20.24999999999999289, 3.550687472877664952 ) ) ;
#550 = CARTESIAN_POINT ( 'NONE',  ( -10.18405858231679595, -21.32873467460644079, 2.757051763020455404 ) ) ;
#551 = VERTEX_POINT ( 'NONE', #2158 ) ;
#552 = CARTESIAN_POINT ( 'NONE',  ( 13.11345185444515415, 3.666818649476655700, 6.750360829155977349 ) ) ;
#553 = EDGE_CURVE ( 'NONE', #4594, #7048, #16384, .T. ) ;
#554 = CARTESIAN_POINT ( 'NONE',  ( 13.09123688038123490, 4.044962459253448550, 5.255034774807352704 ) ) ;
#555 = VECTOR ( 'NONE', #16159, 1000.000000000000000 ) ;
#556 = CARTESIAN_POINT ( 'NONE',  ( 8.126396343307449754, 0.000000000000000000, 1.000000000000000000 ) ) ;
#557 = ORIENTED_EDGE ( 'NONE', *, *, #18497, .T. ) ;
#558 = ORIENTED_EDGE ( 'NONE', *, *, #7385, .F. ) ;
#559 = CARTESIAN_POINT ( 'NONE',  ( 24.50000000000000000, 3.000000000000000888, 1.000000000000000000 ) ) ;
#560 = DIRECTION ( 'NONE',  ( -0.000000000000000000, 0.000000000000000000, -1.000000000000000000 ) ) ;
#561 = CARTESIAN_POINT ( 'NONE',  ( 13.00209451496117374, 11.64110105645932691, 0.000000000000000000 ) ) ;
#562 = CYLINDRICAL_SURFACE ( 'NONE', #14318, 10.00000000000000000 ) ;
#563 = CARTESIAN_POINT ( 'NONE',  ( 3.277163086644854229, -14.76879761173520578, 3.824673233536266537 ) ) ;
#564 = LINE ( 'NONE', #11752, #7741 ) ;
#565 = CARTESIAN_POINT ( 'NONE',  ( 11.99178095869207006, 9.000000000000001776, 1.000000000000000000 ) ) ;
#566 = EDGE_CURVE ( 'NONE', #17379, #995, #898, .T. ) ;
#567 = LINE ( 'NONE', #16465, #6029 ) ;
#568 = CARTESIAN_POINT ( 'NONE',  ( 15.50000000000000178, -20.99999999999999645, 4.000000000000000000 ) ) ;
#569 = CARTESIAN_POINT ( 'NONE',  ( -9.246558582316794173, -21.94931252712234482, 5.250000000000000888 ) ) ;
#570 = EDGE_CURVE ( 'NONE', #2226, #5682, #13143, .T. ) ;
#571 = CARTESIAN_POINT ( 'NONE',  ( -3.451187703687236041, -10.75258211228477734, 2.985843844067104680 ) ) ;
#572 = ORIENTED_EDGE ( 'NONE', *, *, #19968, .T. ) ;
#573 = CARTESIAN_POINT ( 'NONE',  ( -13.09560269887985307, 4.265436293439658577, 4.973800642626965640 ) ) ;
#574 = LINE ( 'NONE', #19934, #13378 ) ;
#575 = CARTESIAN_POINT ( 'NONE',  ( -5.409691417683178294, -21.32581373872474373, 5.270995438708348857 ) ) ;
#576 = ORIENTED_EDGE ( 'NONE', *, *, #19487, .F. ) ;
#577 = CARTESIAN_POINT ( 'NONE',  ( 13.39169183355864590, -18.65706240528901105, 4.755687463382285429 ) ) ;
#578 = CARTESIAN_POINT ( 'NONE',  ( 1.811130159782011528, 0.000000000000000000, 1.000000000000000000 ) ) ;
#579 = ORIENTED_EDGE ( 'NONE', *, *, #13507, .T. ) ;
#580 = ORIENTED_EDGE ( 'NONE', *, *, #14379, .F. ) ;
#581 = CARTESIAN_POINT ( 'NONE',  ( 15.50000000000000178, -23.00000000000000711, 1.000000000000000000 ) ) ;
#582 = ORIENTED_EDGE ( 'NONE', *, *, #16071, .F. ) ;
#583 = CARTESIAN_POINT ( 'NONE',  ( -3.500698171653725765, 11.64110105645932691, 0.000000000000000000 ) ) ;
#584 = VECTOR ( 'NONE', #15881, 1000.000000000000000 ) ;
#585 = EDGE_LOOP ( 'NONE', ( #6013, #20660, #8946, #16986 ) ) ;
#586 = DIRECTION ( 'NONE',  ( 0.000000000000000000, 1.000000000000000000, -0.000000000000000000 ) ) ;
#587 = PLANE ( 'NONE',  #2307 ) ;
#588 = LINE ( 'NONE', #19745, #15656 ) ;
#589 = CARTESIAN_POINT ( 'NONE',  ( 1.728780693989796724, -8.364929292255887106, 2.372646901726390478 ) ) ;
#590 = CARTESIAN_POINT ( 'NONE',  ( -5.965308582316793284, -20.22900456129164937, 4.174186261275266929 ) ) ;
#591 = ADVANCED_FACE ( 'NONE', ( #6870 ), #5194, .F. ) ;
#592 = CARTESIAN_POINT ( 'NONE',  ( 12.66863463945108137, -18.79645070772368953, 6.267287912489321045 ) ) ;
#593 = DIRECTION ( 'NONE',  ( 0.000000000000000000, 1.000000000000000000, -0.000000000000000000 ) ) ;
#594 = EDGE_CURVE ( 'NONE', #13481, #20714, #588, .T. ) ;
#595 = CARTESIAN_POINT ( 'NONE',  ( 4.284691417683176518, -23.77099543870834353, 4.174186261275252718 ) ) ;
#596 = CARTESIAN_POINT ( 'NONE',  ( 11.00000000000000000, -18.49999999999999645, 6.500000000000000888 ) ) ;
#597 = CARTESIAN_POINT ( 'NONE',  ( -9.628441417683177406, -20.99999999999999645, 3.550687472877664952 ) ) ;
#598 = CARTESIAN_POINT ( 'NONE',  ( -6.434058582316796837, -23.73192549717337130, 5.303608408759367343 ) ) ;
#599 = EDGE_LOOP ( 'NONE', ( #16407, #1610, #13461, #14948 ) ) ;
#600 = CARTESIAN_POINT ( 'NONE',  ( 12.79798428357658047, -11.51429367935891790, 5.673858176248284479 ) ) ;
#601 = CARTESIAN_POINT ( 'NONE',  ( -13.11345185444515415, 3.666818649476655700, 6.750360829155977349 ) ) ;
#602 = ORIENTED_EDGE ( 'NONE', *, *, #19126, .F. ) ;
#603 = DIRECTION ( 'NONE',  ( 5.204170427930411817E-15, -1.000000000000000000, 0.000000000000000000 ) ) ;
#604 = LINE ( 'NONE', #15142, #17681 ) ;
#605 = ORIENTED_EDGE ( 'NONE', *, *, #19738, .F. ) ;
#606 = SHAPE_DEFINITION_REPRESENTATION ( #14520, #19662 ) ;
#607 = VERTEX_POINT ( 'NONE', #11775 ) ;
#608 = EDGE_CURVE ( 'NONE', #4592, #5966, #18167, .T. ) ;
#609 = CARTESIAN_POINT ( 'NONE',  ( 12.79327455738548203, -19.93647458090189772, 3.527980527292456259 ) ) ;
#610 = VERTEX_POINT ( 'NONE', #19851 ) ;
#611 = DIRECTION ( 'NONE',  ( 1.000000000000000000, 0.000000000000000000, 0.000000000000000000 ) ) ;
#612 = CARTESIAN_POINT ( 'NONE',  ( 0.000000000000000000, -9.114917468222230923, 1.622643865078341019 ) ) ;
#613 = AXIS2_PLACEMENT_3D ( 'NONE', #19953, #11673, #2065 ) ;
#614 = CARTESIAN_POINT ( 'NONE',  ( -1.960495238260606010, -8.383787449798761671, 1.627490053312942164 ) ) ;
#615 = CARTESIAN_POINT ( 'NONE',  ( -8.376396343307449754, 11.64110105645932691, 10.00000000000000000 ) ) ;
#616 = LINE ( 'NONE', #726, #14849 ) ;
#617 = PLANE ( 'NONE',  #15078 ) ;
#618 = CARTESIAN_POINT ( 'NONE',  ( 21.67243175760212637, 9.000000000000001776, 1.000000000000000000 ) ) ;
#619 = CARTESIAN_POINT ( 'NONE',  ( 9.527808582316795949, -24.47900456129166358, 4.586221378810390270 ) ) ;
#620 = CARTESIAN_POINT ( 'NONE',  ( -13.12405442816082868, 4.202248622120948518, 6.747400073346936367 ) ) ;
#621 = CARTESIAN_POINT ( 'NONE',  ( -7.472191417683177406, -24.47900456129165292, 2.413778621189595963 ) ) ;
#622 = FACE_OUTER_BOUND ( 'NONE', #5655, .T. ) ;
#623 = DIRECTION ( 'NONE',  ( 0.000000000000000000, 1.000000000000000000, 0.000000000000000000 ) ) ;
#624 = VECTOR ( 'NONE', #19202, 1000.000000000000000 ) ;
#625 = VECTOR ( 'NONE', #15350, 1000.000000000000000 ) ;
#626 = CARTESIAN_POINT ( 'NONE',  ( 6.996558582316795949, -22.05068747287764452, 2.499999999999999112 ) ) ;
#627 = CARTESIAN_POINT ( 'NONE',  ( 0.000000000000000000, 4.999999999999999112, 1.000000000000000000 ) ) ;
#628 = VECTOR ( 'NONE', #3098, 1000.000000000000000 ) ;
#629 = ORIENTED_EDGE ( 'NONE', *, *, #10847, .F. ) ;
#630 = ORIENTED_EDGE ( 'NONE', *, *, #4807, .F. ) ;
#631 = CARTESIAN_POINT ( 'NONE',  ( 13.49014615398506045, -14.43511922376608680, 5.596513032956658584 ) ) ;
#632 = CARTESIAN_POINT ( 'NONE',  ( -20.92243175760212637, 9.000000000000001776, 1.000000000000000000 ) ) ;
#633 = ORIENTED_EDGE ( 'NONE', *, *, #1622, .T. ) ;
#634 = CARTESIAN_POINT ( 'NONE',  ( 4.000698171653723101, 10.00000000000000000, 1.000000000000000000 ) ) ;
#635 = CARTESIAN_POINT ( 'NONE',  ( -7.500000000000000000, -23.83493649053891517, 4.999999999999999112 ) ) ;
#636 = LINE ( 'NONE', #7026, #13982 ) ;
#637 = ADVANCED_FACE ( 'NONE', ( #5502 ), #2365, .F. ) ;
#638 = CARTESIAN_POINT ( 'NONE',  ( 13.37515323800563039, -20.24226148071262799, 4.627790572011877934 ) ) ;
#639 = AXIS2_PLACEMENT_3D ( 'NONE', #157, #12701, #9776 ) ;
#640 = CARTESIAN_POINT ( 'NONE',  ( -5.999999999999999112, -7.500000000000047073, 2.000000000000000000 ) ) ;
#641 = CARTESIAN_POINT ( 'NONE',  ( 0.000000000000000000, -8.364917468222230923, 2.372643865078341019 ) ) ;
#642 = VECTOR ( 'NONE', #3133, 1000.000000000000000 ) ;
#643 = LINE ( 'NONE', #752, #2713 ) ;
#644 = CARTESIAN_POINT ( 'NONE',  ( -12.62562661273123332, -19.46835605706984040, 4.628101975944573176 ) ) ;
#645 = CARTESIAN_POINT ( 'NONE',  ( 4.840308582316793284, -22.67418626127525982, 5.270995438708342640 ) ) ;
#646 = CARTESIAN_POINT ( 'NONE',  ( 23.10856191738414012, 9.000000000000001776, 1.000000000000000000 ) ) ;
#647 = CARTESIAN_POINT ( 'NONE',  ( 12.91308523408712183, -5.701695678577235249, 5.798858176249892082 ) ) ;
#648 = CARTESIAN_POINT ( 'NONE',  ( -1.668644041176298387, -9.864915931696323526, 2.372643470467795890 ) ) ;
#649 = CARTESIAN_POINT ( 'NONE',  ( 10.74655858231679595, -21.94931252712234127, 4.499999999999999112 ) ) ;
#650 = CARTESIAN_POINT ( 'NONE',  ( 11.87844141768317563, -23.74999999999999645, 3.449312527122335492 ) ) ;
#651 = CARTESIAN_POINT ( 'NONE',  ( -7.934058582316792396, -23.20159541128345992, 4.773278322869455970 ) ) ;
#652 = ORIENTED_EDGE ( 'NONE', *, *, #14971, .T. ) ;
#653 = CARTESIAN_POINT ( 'NONE',  ( 13.12175473207386922, 4.086113969730903683, 6.756475741440692850 ) ) ;
#654 = CARTESIAN_POINT ( 'NONE',  ( 12.62500797102436678, -19.49959746326937093, 4.516621614626514791 ) ) ;
#655 = ORIENTED_EDGE ( 'NONE', *, *, #12607, .T. ) ;
#656 = AXIS2_PLACEMENT_3D ( 'NONE', #3159, #9531, #15903 ) ;
#657 = ORIENTED_EDGE ( 'NONE', *, *, #3638, .T. ) ;
#658 = DIRECTION ( 'NONE',  ( -1.000000000000000000, 0.000000000000000000, 0.000000000000000000 ) ) ;
#659 = AXIS2_PLACEMENT_3D ( 'NONE', #17311, #5726, #12097 ) ;
#660 = VECTOR ( 'NONE', #4913, 1000.000000000000000 ) ;
#661 = EDGE_CURVE ( 'NONE', #485, #9583, #9261, .T. ) ;
#662 = DIRECTION ( 'NONE',  ( 1.000000000000000000, 0.000000000000000000, 0.000000000000000000 ) ) ;
#663 = CARTESIAN_POINT ( 'NONE',  ( -26.94203811574920593, 0.000000000000000000, 0.000000000000000000 ) ) ;
#664 = EDGE_CURVE ( 'NONE', #12892, #14133, #14065, .T. ) ;
#665 = DIRECTION ( 'NONE',  ( 1.000000000000000000, 0.000000000000000000, -0.000000000000000000 ) ) ;
#666 = CARTESIAN_POINT ( 'NONE',  ( 1.772926875221950249, -9.883376166076789815, 2.377384427436886494 ) ) ;
#667 = DIRECTION ( 'NONE',  ( 1.000000000000000000, 0.000000000000000000, -0.000000000000000000 ) ) ;
#668 = VECTOR ( 'NONE', #922, 1000.000000000000000 ) ;
#669 = EDGE_CURVE ( 'NONE', #13945, #9626, #15323, .T. ) ;
#670 = DIRECTION ( 'NONE',  ( 0.000000000000000000, 1.000000000000000000, -0.000000000000000000 ) ) ;
#671 = DIRECTION ( 'NONE',  ( -1.000000000000000000, 0.000000000000000000, -0.000000000000000000 ) ) ;
#672 = PRESENTATION_LAYER_ASSIGNMENT (  '', '', ( #17034 ) ) ;
#673 = PLANE ( 'NONE',  #282 ) ;
#674 = CARTESIAN_POINT ( 'NONE',  ( -6.809058582316794173, -23.27327832286945153, 2.298404588716537411 ) ) ;
#675 = CARTESIAN_POINT ( 'NONE',  ( -3.502569552650398155, -9.961070227720959736, 2.032567780072621400 ) ) ;
#676 = ORIENTED_EDGE ( 'NONE', *, *, #19705, .T. ) ;
#677 = VECTOR ( 'NONE', #10798, 1000.000000000000000 ) ;
#678 = CARTESIAN_POINT ( 'NONE',  ( -13.37499999999998224, -19.49999999999998934, 4.166666666666637653 ) ) ;
#679 = CARTESIAN_POINT ( 'NONE',  ( -4.840308582316793284, -22.67418626127525982, 5.270995438708342640 ) ) ;
#680 = CIRCLE ( 'NONE', #7376, 10.00000000000000000 ) ;
#681 = CARTESIAN_POINT ( 'NONE',  ( -11.40969141768317918, -21.63647391050456648, 4.520995438708348857 ) ) ;
#682 = VERTEX_POINT ( 'NONE', #12399 ) ;
#683 = CARTESIAN_POINT ( 'NONE',  ( 13.39542766346049518, -19.21840299524461315, 5.493648449623241170 ) ) ;
#684 = DIRECTION ( 'NONE',  ( 0.000000000000000000, 1.000000000000000000, -0.000000000000000000 ) ) ;
#685 = ORIENTED_EDGE ( 'NONE', *, *, #6597, .T. ) ;
#686 = ORIENTED_EDGE ( 'NONE', *, *, #20030, .T. ) ;
#687 = LINE ( 'NONE', #13638, #17158 ) ;
#688 = EDGE_LOOP ( 'NONE', ( #8301, #4160, #16182, #17775 ) ) ;
#689 = CARTESIAN_POINT ( 'NONE',  ( -13.37499999999998579, -20.24999999999999289, 3.666666666666653640 ) ) ;
#690 = EDGE_CURVE ( 'NONE', #11466, #16861, #9064, .T. ) ;
#691 = AXIS2_PLACEMENT_3D ( 'NONE', #3479, #1908, #9120 ) ;
#692 = ORIENTED_EDGE ( 'NONE', *, *, #16527, .T. ) ;
#693 = DIRECTION ( 'NONE',  ( 1.000000000000000000, 0.000000000000000000, 0.000000000000000000 ) ) ;
#694 = CARTESIAN_POINT ( 'NONE',  ( -14.49999999999998579, -18.49999999999999645, 4.000000000000000000 ) ) ;
#695 = VECTOR ( 'NONE', #5802, 1000.000000000000000 ) ;
#696 = VECTOR ( 'NONE', #19733, 1000.000000000000000 ) ;
#697 = FACE_OUTER_BOUND ( 'NONE', #48, .T. ) ;
#698 = CARTESIAN_POINT ( 'NONE',  ( 3.173374397671306912, -9.279487642487616483, 2.607523756204581211 ) ) ;
#699 = CARTESIAN_POINT ( 'NONE',  ( -7.371558582316794173, -20.24999999999999289, 3.449312527122348371 ) ) ;
#700 = CARTESIAN_POINT ( 'NONE',  ( 12.62927505847832776, -20.78410954684871825, 5.373974324164845662 ) ) ;
#701 = B_SPLINE_CURVE_WITH_KNOTS ( 'NONE', 3,
 ( #1316, #14061, #7896, #20471, #12592, #14258 ),
 .UNSPECIFIED., .F., .F.,
 ( 4, 2, 4 ),
 ( 0.5000000000000000000, 0.7500000000000000000, 1.000000000000000000 ),
 .UNSPECIFIED. ) ;
#702 = PLANE ( 'NONE',  #15627 ) ;
#703 = CARTESIAN_POINT ( 'NONE',  ( 4.472191417683177406, -23.72900456129165292, 2.724438792969417822 ) ) ;
#704 = DIRECTION ( 'NONE',  ( -0.000000000000000000, -0.000000000000000000, -1.000000000000000000 ) ) ;
#705 = CARTESIAN_POINT ( 'NONE',  ( -4.472191417683178294, -22.97900456129165292, 3.035098964749240125 ) ) ;
#706 = CARTESIAN_POINT ( 'NONE',  ( -5.590308582316795949, -21.01515356694490322, 0.9790045612916562501 ) ) ;
#707 = ORIENTED_EDGE ( 'NONE', *, *, #15426, .F. ) ;
#708 = CARTESIAN_POINT ( 'NONE',  ( 12.62499999999998401, -19.49999999999998934, 3.666666666666654084 ) ) ;
#709 = CARTESIAN_POINT ( 'NONE',  ( -13.09532840572934376, 3.501584489333809724, 5.996774842915142401 ) ) ;
#710 = ORIENTED_EDGE ( 'NONE', *, *, #2316, .F. ) ;
#711 = AXIS2_PLACEMENT_3D ( 'NONE', #20236, #7367, #5796 ) ;
#712 = CARTESIAN_POINT ( 'NONE',  ( 22.56633994409548194, 16.00000000000000000, 1.000000000000000000 ) ) ;
#713 = CARTESIAN_POINT ( 'NONE',  ( 27.52582389412042474, 4.853545418763153485, 0.000000000000000000 ) ) ;
#714 = AXIS2_PLACEMENT_3D ( 'NONE', #5891, #15604, #12261 ) ;
#715 = ORIENTED_EDGE ( 'NONE', *, *, #12942, .T. ) ;
#716 = VECTOR ( 'NONE', #3309, 1000.000000000000000 ) ;
#717 = ORIENTED_EDGE ( 'NONE', *, *, #19240, .F. ) ;
#718 = EDGE_CURVE ( 'NONE', #4809, #5545, #7592, .T. ) ;
#719 = FACE_OUTER_BOUND ( 'NONE', #15342, .T. ) ;
#720 = EDGE_CURVE ( 'NONE', #9416, #11125, #2883, .T. ) ;
#721 = ORIENTED_EDGE ( 'NONE', *, *, #19909, .T. ) ;
#722 = CARTESIAN_POINT ( 'NONE',  ( 4.000000000000000000, -12.50000000000000000, 1.000000000000000000 ) ) ;
#723 = CARTESIAN_POINT ( 'NONE',  ( 13.08094078691552831, 2.775009739235173356, 5.981149842915306714 ) ) ;
#724 = CARTESIAN_POINT ( 'NONE',  ( -3.486710468562268961, -9.848741751643258269, 2.003719583429115492 ) ) ;
#725 = DIRECTION ( 'NONE',  ( -0.000000000000000000, 0.000000000000000000, -1.000000000000000000 ) ) ;
#726 = CARTESIAN_POINT ( 'NONE',  ( -20.75349085826862350, 10.00000000000000000, 1.000000000000000000 ) ) ;
#727 = VECTOR ( 'NONE', #14197, 1000.000000000000000 ) ;
#728 = CARTESIAN_POINT ( 'NONE',  ( 0.000000000000000000, 4.999999999999999112, 0.000000000000000000 ) ) ;
#729 = DIRECTION ( 'NONE',  ( 0.000000000000000000, 1.000000000000000000, -0.000000000000000000 ) ) ;
#730 = CARTESIAN_POINT ( 'NONE',  ( 10.00344141768317741, -22.05068747287766229, 6.000000000000001776 ) ) ;
#731 = CARTESIAN_POINT ( 'NONE',  ( -12.63465172146706728, -19.76258806590802664, 5.372658420469845986 ) ) ;
#732 = EDGE_CURVE ( 'NONE', #15336, #11328, #16999, .T. ) ;
#733 = CARTESIAN_POINT ( 'NONE',  ( -5.315941417683176518, -20.26807450282663225, 5.303608408759377113 ) ) ;
#734 = VERTEX_POINT ( 'NONE', #2564 ) ;
#735 = CARTESIAN_POINT ( 'NONE',  ( 7.499999999999999112, -18.49999999999999645, 6.500000000000000888 ) ) ;
#736 = DIRECTION ( 'NONE',  ( 0.000000000000000000, 0.1264857625231113059, 0.9919684228235025047 ) ) ;
#737 = CARTESIAN_POINT ( 'NONE',  ( -13.77789853026076550, 0.09637577819625635367, 5.909013032956687006 ) ) ;
#738 = CARTESIAN_POINT ( 'NONE',  ( 7.465308582316796837, -20.97900456129165647, 3.863526089495444626 ) ) ;
#739 = CARTESIAN_POINT ( 'NONE',  ( -14.49999999999998579, -25.49999999999999645, 1.000000000000000000 ) ) ;
#740 = VERTEX_POINT ( 'NONE', #20055 ) ;
#741 = EDGE_LOOP ( 'NONE', ( #10887, #4261, #18676, #2268, #15145, #1206, #20181, #1106, #10536, #17693, #14548, #16300, #9153, #18986 ) ) ;
#742 = CARTESIAN_POINT ( 'NONE',  ( 13.87444723674697755, 4.972085455720938185, 5.163895512850782410 ) ) ;
#743 = DIRECTION ( 'NONE',  ( 0.000000000000000000, 0.000000000000000000, 1.000000000000000000 ) ) ;
#744 = ORIENTED_EDGE ( 'NONE', *, *, #16763, .T. ) ;
#745 = AXIS2_PLACEMENT_3D ( 'NONE', #893, #13543, #3828 ) ;
#746 = CARTESIAN_POINT ( 'NONE',  ( 0.000000000000000000, 4.999999999999999112, 0.000000000000000000 ) ) ;
#747 = DIRECTION ( 'NONE',  ( 0.000000000000000000, -0.000000000000000000, 1.000000000000000000 ) ) ;
#748 = DIRECTION ( 'NONE',  ( 0.000000000000000000, 0.000000000000000000, -1.000000000000000000 ) ) ;
#749 = CARTESIAN_POINT ( 'NONE',  ( 13.41820805991576826, -18.06799297425606454, 5.518388032956592859 ) ) ;
#750 = DIRECTION ( 'NONE',  ( 0.000000000000000000, 0.000000000000000000, 1.000000000000000000 ) ) ;
#751 = CARTESIAN_POINT ( 'NONE',  ( 1.957016269584227031, -9.152392576945766578, 2.382268221639079364 ) ) ;
#752 = CARTESIAN_POINT ( 'NONE',  ( -2.981555974335140152E-16, 2.500000000000002220, 2.000000000000000000 ) ) ;
#753 = CARTESIAN_POINT ( 'NONE',  ( -12.62499999999998224, -19.50000000000006040, 4.416666666666682062 ) ) ;
#754 = PRESENTATION_STYLE_ASSIGNMENT (( #11425 ) ) ;
#755 = CARTESIAN_POINT ( 'NONE',  ( 12.43405858231679417, -23.20159541128345992, 4.773278322869455970 ) ) ;
#756 = CARTESIAN_POINT ( 'NONE',  ( -13.79242507427300879, 0.07996625081441015304, 6.658692769197546824 ) ) ;
#757 = VECTOR ( 'NONE', #16963, 1000.000000000000000 ) ;
#758 = ADVANCED_FACE ( 'NONE', ( #4458 ), #15434, .T. ) ;
#759 = LINE ( 'NONE', #1071, #677 ) ;
#760 = CARTESIAN_POINT ( 'NONE',  ( 8.215308582316795949, -23.02099543870833998, 3.136473910504556262 ) ) ;
#761 = CARTESIAN_POINT ( 'NONE',  ( 8.878441417683177406, -23.74999999999999645, 3.449312527122335492 ) ) ;
#762 = CARTESIAN_POINT ( 'NONE',  ( -11.30905858231679417, -23.27327832286945153, 2.298404588716537411 ) ) ;
#763 = ORIENTED_EDGE ( 'NONE', *, *, #6414, .F. ) ;
#764 = CARTESIAN_POINT ( 'NONE',  ( 12.66204031416134335, -19.12946413485185104, 6.260126454156002218 ) ) ;
#765 = CARTESIAN_POINT ( 'NONE',  ( 13.08799567112409790, 3.881281391764801025, 5.254907606674271037 ) ) ;
#766 = FACE_OUTER_BOUND ( 'NONE', #18789, .T. ) ;
#767 = ORIENTED_EDGE ( 'NONE', *, *, #8340, .T. ) ;
#768 = ORIENTED_EDGE ( 'NONE', *, *, #15761, .T. ) ;
#769 = DIRECTION ( 'NONE',  ( -0.000000000000000000, -0.000000000000000000, -1.000000000000000000 ) ) ;
#770 = VECTOR ( 'NONE', #17153, 1000.000000000000000 ) ;
#771 = CARTESIAN_POINT ( 'NONE',  ( 16.37779268661489596, 0.000000000000000000, 1.000000000000000000 ) ) ;
#772 = DIRECTION ( 'NONE',  ( 0.000000000000000000, -0.000000000000000000, -1.000000000000000000 ) ) ;
#773 = CARTESIAN_POINT ( 'NONE',  ( 20.50349085826861995, 0.000000000000000000, 0.000000000000000000 ) ) ;
#774 = CARTESIAN_POINT ( 'NONE',  ( 1.824218240560544047, -9.921717538097572842, 2.387231257717697286 ) ) ;
#775 = DIRECTION ( 'NONE',  ( 0.000000000000000000, 0.000000000000000000, 1.000000000000000000 ) ) ;
#776 = LINE ( 'NONE', #10288, #15723 ) ;
#777 = DIRECTION ( 'NONE',  ( 1.000000000000000000, 0.000000000000000000, 0.000000000000000000 ) ) ;
#778 = CARTESIAN_POINT ( 'NONE',  ( -25.29469207716615031, 9.000000000000001776, 1.000000000000000000 ) ) ;
#779 = CARTESIAN_POINT ( 'NONE',  ( -4.934058582316793284, -23.20159541128345992, 4.773278322869455970 ) ) ;
#780 = CARTESIAN_POINT ( 'NONE',  ( -0.9854920305337622199, -8.364917468222230923, 2.372643865078341019 ) ) ;
#781 = ORIENTED_EDGE ( 'NONE', *, *, #10378, .T. ) ;
#782 = CARTESIAN_POINT ( 'NONE',  ( -13.37500000000002132, -19.49999999999450040, 3.833333333368183382 ) ) ;
#783 = CARTESIAN_POINT ( 'NONE',  ( -7.652808582316795061, -21.22443879296942626, 5.229004561291659137 ) ) ;
#784 = EDGE_CURVE ( 'NONE', #4291, #411, #2676, .T. ) ;
#785 = CARTESIAN_POINT ( 'NONE',  ( 11.40280858231679595, -23.08622137881038938, 1.020995438708339309 ) ) ;
#786 = CARTESIAN_POINT ( 'NONE',  ( -9.065941417683177406, -22.67126532539353789, 2.757051763020445634 ) ) ;
#787 = ORIENTED_EDGE ( 'NONE', *, *, #12469, .F. ) ;
#788 = CARTESIAN_POINT ( 'NONE',  ( 13.37597619100657198, -20.20070235416671167, 4.815535977982682070 ) ) ;
#789 = CARTESIAN_POINT ( 'NONE',  ( -27.94203811574922725, 3.231447299068595019E-14, 1.000000000000000000 ) ) ;
#790 = ORIENTED_EDGE ( 'NONE', *, *, #9633, .T. ) ;
#791 = ORIENTED_EDGE ( 'NONE', *, *, #13338, .F. ) ;
#792 = LINE ( 'NONE', #7177, #1752 ) ;
#793 = ORIENTED_EDGE ( 'NONE', *, *, #7303, .T. ) ;
#794 = LINE ( 'NONE', #11664, #1088 ) ;
#795 = EDGE_CURVE ( 'NONE', #20584, #14806, #3312, .T. ) ;
#796 = EDGE_CURVE ( 'NONE', #3716, #11889, #6025, .T. ) ;
#797 = VECTOR ( 'NONE', #17296, 1000.000000000000000 ) ;
#798 = ORIENTED_EDGE ( 'NONE', *, *, #5836, .F. ) ;
#799 = FACE_OUTER_BOUND ( 'NONE', #12254, .T. ) ;
#800 = PLANE ( 'NONE',  #12000 ) ;
#801 = DIRECTION ( 'NONE',  ( 0.000000000000000000, 0.000000000000000000, 1.000000000000000000 ) ) ;
#802 = CARTESIAN_POINT ( 'NONE',  ( 0.2815691515810352374, -8.364917468222230923, 2.372643865078523540 ) ) ;
#803 = CARTESIAN_POINT ( 'NONE',  ( -8.496558582316794173, -22.05068747287764452, 1.749999999999998446 ) ) ;
#804 = CARTESIAN_POINT ( 'NONE',  ( 12.62672826945118665, -20.91272239271162903, 5.058631648758789900 ) ) ;
#805 = CARTESIAN_POINT ( 'NONE',  ( -18.69064177244175795, 11.64110105645932691, 10.00000000000000000 ) ) ;
#806 = CARTESIAN_POINT ( 'NONE',  ( 11.59719141768317741, -22.46490103525075810, 4.479004561291653808 ) ) ;
#807 = CARTESIAN_POINT ( 'NONE',  ( -13.67791111847408025, 4.999999999999999112, 0.000000000000000000 ) ) ;
#808 = CARTESIAN_POINT ( 'NONE',  ( -4.097191417683177406, -22.46490103525075810, 4.479004561291653808 ) ) ;
#809 = EDGE_CURVE ( 'NONE', #15986, #11334, #18580, .T. ) ;
#810 = CARTESIAN_POINT ( 'NONE',  ( -4.717959273841179524, -21.63341328858655999, 5.993595146365859883 ) ) ;
#811 = ORIENTED_EDGE ( 'NONE', *, *, #14623, .T. ) ;
#812 = CARTESIAN_POINT ( 'NONE',  ( 13.11740841389447709, 4.616624901677048420, 5.813473370769506765 ) ) ;
#813 = CARTESIAN_POINT ( 'NONE',  ( -13.08094078691552831, 2.775009739235173356, 5.981149842915306714 ) ) ;
#814 = VERTEX_POINT ( 'NONE', #10623 ) ;
#815 = LINE ( 'NONE', #7299, #19326 ) ;
#816 = DIRECTION ( 'NONE',  ( -0.000000000000000000, 0.000000000000000000, -1.000000000000000000 ) ) ;
#817 = EDGE_LOOP ( 'NONE', ( #11943, #5676, #6063, #12462 ) ) ;
#818 = ITEM_DEFINED_TRANSFORMATION ( 'NONE', 'NONE', #18060,  #18039 ) ;
#819 = ORIENTED_EDGE ( 'NONE', *, *, #12042, .F. ) ;
#820 = ORIENTED_EDGE ( 'NONE', *, *, #2735, .F. ) ;
#821 = EDGE_CURVE ( 'NONE', #7330, #19819, #20258, .T. ) ;
#822 = CARTESIAN_POINT ( 'NONE',  ( -2.693754455098655409, -10.04853567022903782, 2.237415670251142519 ) ) ;
#823 = LINE ( 'NONE', #10649, #7633 ) ;
#824 = CARTESIAN_POINT ( 'NONE',  ( -3.506783328160878010, -9.991161114504492957, 2.040295720924476530 ) ) ;
#825 = DIRECTION ( 'NONE',  ( 1.000000000000000000, 0.000000000000000000, -0.000000000000000000 ) ) ;
#826 = CARTESIAN_POINT ( 'NONE',  ( 2.311130159782011972, 4.999999999999999112, 0.000000000000000000 ) ) ;
#827 = CARTESIAN_POINT ( 'NONE',  ( -11.24178095869206828, 9.000000000000001776, 1.000000000000000000 ) ) ;
#828 = CARTESIAN_POINT ( 'NONE',  ( 6.340308582316796837, -22.98484643305508612, 6.020995438708344416 ) ) ;
#829 = CARTESIAN_POINT ( 'NONE',  ( -13.12512971825177033, 5.006550771716304915, 5.133277049491872468 ) ) ;
#830 = CARTESIAN_POINT ( 'NONE',  ( -8.972191417683177406, -24.47900456129165292, 2.413778621189595963 ) ) ;
#831 = ADVANCED_FACE ( 'NONE', ( #10843 ), #17206, .F. ) ;
#832 = ORIENTED_EDGE ( 'NONE', *, *, #2086, .F. ) ;
#833 = ADVANCED_FACE ( 'NONE', ( #17106 ), #10937, .T. ) ;
#834 = CARTESIAN_POINT ( 'NONE',  ( 12.80905858231679417, -23.27327832286945153, 2.298404588716537411 ) ) ;
#835 = DIRECTION ( 'NONE',  ( 1.000000000000000000, -0.000000000000000000, 0.000000000000000000 ) ) ;
#836 = CARTESIAN_POINT ( 'NONE',  ( -13.39782821820594627, -19.84717498059871943, 6.143582220458365661 ) ) ;
#837 = CARTESIAN_POINT ( 'NONE',  ( 12.99655858231679417, -22.05068747287764452, 1.749999999999998446 ) ) ;
#838 = CARTESIAN_POINT ( 'NONE',  ( -11.00000000000000000, -19.49999999999999645, 5.000000000000000000 ) ) ;
#839 = ORIENTED_EDGE ( 'NONE', *, *, #13617, .T. ) ;
#840 = ORIENTED_EDGE ( 'NONE', *, *, #2595, .T. ) ;
#841 = CARTESIAN_POINT ( 'NONE',  ( 13.77789853026076550, 0.09637577819625635367, 5.909013032956687006 ) ) ;
#842 = VECTOR ( 'NONE', #18531, 1000.000000000000000 ) ;
#843 = DIRECTION ( 'NONE',  ( 0.000000000000000000, 1.000000000000000000, 0.000000000000000000 ) ) ;
#844 = FILL_AREA_STYLE ('',( #8584 ) ) ;
#845 = ORIENTED_EDGE ( 'NONE', *, *, #9874, .T. ) ;
#846 = LINE ( 'NONE', #4289, #16135 ) ;
#847 = DIRECTION ( 'NONE',  ( -0.000000000000000000, -0.000000000000000000, -1.000000000000000000 ) ) ;
#848 = DIRECTION ( 'NONE',  ( 1.000000000000000000, 0.000000000000000000, 0.000000000000000000 ) ) ;
#849 = CARTESIAN_POINT ( 'NONE',  ( -9.000000000000000000, -9.999999999999992895, 2.500000000000000000 ) ) ;
#850 = CARTESIAN_POINT ( 'NONE',  ( -2.187849085826861550, 10.00000000000000000, 1.000000000000000000 ) ) ;
#851 = CARTESIAN_POINT ( 'NONE',  ( 3.636036383999129207, -10.90885478516162976, 2.275977788322152584 ) ) ;
#852 = CARTESIAN_POINT ( 'NONE',  ( -13.87470602645761808, 4.985154336109792972, 4.000000000000000000 ) ) ;
#853 = CARTESIAN_POINT ( 'NONE',  ( -12.65396917024039958, -18.03705690286155772, 4.783553440007634272 ) ) ;
#854 = FACE_OUTER_BOUND ( 'NONE', #19395, .T. ) ;
#855 = AXIS2_PLACEMENT_3D ( 'NONE', #14509, #8242, #12934 ) ;
#856 = CARTESIAN_POINT ( 'NONE',  ( -0.000000000000000000, 10.00000000000000000, 0.000000000000000000 ) ) ;
#857 = CARTESIAN_POINT ( 'NONE',  ( -13.87470602645761986, 4.985154336109792972, 3.000000000000000000 ) ) ;
#858 = EDGE_CURVE ( 'NONE', #20067, #12385, #1217, .T. ) ;
#859 = DIRECTION ( 'NONE',  ( -1.000000000000000000, 0.000000000000000000, 0.000000000000000000 ) ) ;
#860 = CARTESIAN_POINT ( 'NONE',  ( 13.09030858231679417, -21.32581373872472597, 1.729004561291657582 ) ) ;
#861 = CARTESIAN_POINT ( 'NONE',  ( 9.159691417683175629, -22.36352608949543352, 2.479004561291652031 ) ) ;
#862 = CARTESIAN_POINT ( 'NONE',  ( -9.621558582316794173, -23.74999999999999645, 3.550687472877651629 ) ) ;
#863 = ORIENTED_EDGE ( 'NONE', *, *, #1373, .F. ) ;
#864 = CARTESIAN_POINT ( 'NONE',  ( 12.68302225826488616, -18.06987595762608478, 6.282912912489355683 ) ) ;
#865 = CARTESIAN_POINT ( 'NONE',  ( 12.82182472306881671, -9.560351485048736109, 4.965845106672846399 ) ) ;
#866 = DIRECTION ( 'NONE',  ( 0.000000000000000000, -0.000000000000000000, 1.000000000000000000 ) ) ;
#867 = EDGE_LOOP ( 'NONE', ( #4255, #16725 ) ) ;
#868 = VERTEX_POINT ( 'NONE', #2989 ) ;
#869 = CARTESIAN_POINT ( 'NONE',  ( 10.05565079891005631, 4.999999999999999112, 1.000000000000000000 ) ) ;
#870 = VECTOR ( 'NONE', #16492, 1000.000000000000000 ) ;
#871 = EDGE_CURVE ( 'NONE', #1300, #20320, #11999, .T. ) ;
#872 = CARTESIAN_POINT ( 'NONE',  ( -27.00000000000000000, 0.000000000000000000, 1.000000000000000000 ) ) ;
#873 = DIRECTION ( 'NONE',  ( 1.000000000000000000, 0.000000000000000000, 0.000000000000000000 ) ) ;
#874 = CARTESIAN_POINT ( 'NONE',  ( 11.00000000000000000, -24.49999999999999289, 5.000000000000000000 ) ) ;
#875 = CARTESIAN_POINT ( 'NONE',  ( 1.126276606324276619, -9.864917468222230923, 2.372643865078341019 ) ) ;
#876 = CARTESIAN_POINT ( 'NONE',  ( 20.50349085826861995, 0.000000000000000000, 1.000000000000000000 ) ) ;
#877 = CARTESIAN_POINT ( 'NONE',  ( -12.00000000000000000, -25.49999999999998934, 4.000000000000000000 ) ) ;
#878 = CARTESIAN_POINT ( 'NONE',  ( 4.315753587183822404, -21.47141115243053378, 5.558207674221720573 ) ) ;
#879 = CARTESIAN_POINT ( 'NONE',  ( -12.71530858231679417, -24.52099543870834708, 2.515153566944913432 ) ) ;
#880 = CARTESIAN_POINT ( 'NONE',  ( -1.639793706121975614, -8.364901960018411131, 1.622639882261793343 ) ) ;
#881 = ORIENTED_EDGE ( 'NONE', *, *, #13059, .T. ) ;
#882 = CARTESIAN_POINT ( 'NONE',  ( -13.37523871602689596, -19.48794484064217514, 4.577160611493482634 ) ) ;
#883 = CARTESIAN_POINT ( 'NONE',  ( -6.434058582316794173, -23.20159541128345992, 4.773278322869455970 ) ) ;
#884 = CARTESIAN_POINT ( 'NONE',  ( 7.465308582316796837, -19.47900456129164937, 4.484846433055089676 ) ) ;
#885 = CARTESIAN_POINT ( 'NONE',  ( -12.25344141768317741, -21.94931252712233061, 2.499999999999999112 ) ) ;
#886 = VERTEX_POINT ( 'NONE', #6224 ) ;
#887 = CARTESIAN_POINT ( 'NONE',  ( 13.70116456325478893, -3.778689555664588973, 5.825679699621801433 ) ) ;
#888 = LINE ( 'NONE', #10512, #20085 ) ;
#889 = ORIENTED_EDGE ( 'NONE', *, *, #6722, .T. ) ;
#890 = ORIENTED_EDGE ( 'NONE', *, *, #18715, .T. ) ;
#891 = DIRECTION ( 'NONE',  ( -1.000000000000000000, 0.000000000000000000, 0.000000000000000000 ) ) ;
#892 = ORIENTED_EDGE ( 'NONE', *, *, #4514, .T. ) ;
#893 = CARTESIAN_POINT ( 'NONE',  ( 32.65117217603048516, 6.460468870412194420, 0.000000000000000000 ) ) ;
#894 = ORIENTED_EDGE ( 'NONE', *, *, #18955, .F. ) ;
#895 = CARTESIAN_POINT ( 'NONE',  ( -17.05017143803810242, 9.000000000000001776, 1.000000000000000000 ) ) ;
#896 = DIRECTION ( 'NONE',  ( -1.000000000000000000, -0.000000000000000000, -0.000000000000000000 ) ) ;
#897 = ADVANCED_FACE ( 'NONE', ( #7803 ), #12901, .T. ) ;
#898 = LINE ( 'NONE', #2062, #2292 ) ;
#899 = CARTESIAN_POINT ( 'NONE',  ( 1.743623630681728542, -9.116095536440919744, 2.372946416531167557 ) ) ;
#900 = DIRECTION ( 'NONE',  ( 0.000000000000000000, -0.000000000000000000, 1.000000000000000000 ) ) ;
#901 = CARTESIAN_POINT ( 'NONE',  ( 13.88684657106908205, 4.848251838987907014, 6.535242036940271504 ) ) ;
#902 = LINE ( 'NONE', #13241, #9957 ) ;
#903 = CARTESIAN_POINT ( 'NONE',  ( 8.126396343307449754, 11.64110105645932691, 0.000000000000000000 ) ) ;
#904 = CARTESIAN_POINT ( 'NONE',  ( 11.97219141768317918, -22.97900456129165292, 3.035098964749240125 ) ) ;
#905 = CARTESIAN_POINT ( 'NONE',  ( -12.62503117662529739, -20.24842558042254836, 4.565011198945062354 ) ) ;
#906 = CARTESIAN_POINT ( 'NONE',  ( -6.722191417683176518, -21.02099543870834353, 3.964901035250761208 ) ) ;
#907 = CARTESIAN_POINT ( 'NONE',  ( -8.503441417683177406, -22.05068747287766229, 6.000000000000001776 ) ) ;
#908 = ORIENTED_EDGE ( 'NONE', *, *, #5009, .T. ) ;
#909 = CARTESIAN_POINT ( 'NONE',  ( 12.62933427970994238, -19.28111887465110996, 4.754790882998214840 ) ) ;
#910 = CARTESIAN_POINT ( 'NONE',  ( -13.12500000000000178, 5.000000000000047962, 4.000000000000000000 ) ) ;
#911 = VERTEX_POINT ( 'NONE', #11044 ) ;
#912 = LINE ( 'NONE', #5519, #930 ) ;
#913 = FACE_OUTER_BOUND ( 'NONE', #2688, .T. ) ;
#914 = ORIENTED_EDGE ( 'NONE', *, *, #3010, .F. ) ;
#915 = ITEM_DEFINED_TRANSFORMATION ( 'NONE', 'NONE', #19065,  #18039 ) ;
#916 = ORIENTED_EDGE ( 'NONE', *, *, #5151, .T. ) ;
#917 = ORIENTED_EDGE ( 'NONE', *, *, #11391, .F. ) ;
#918 = DIRECTION ( 'NONE',  ( 0.000000000000000000, -0.000000000000000000, 1.000000000000000000 ) ) ;
#919 = FACE_OUTER_BOUND ( 'NONE', #16776, .T. ) ;
#920 = ADVANCED_FACE ( 'NONE', ( #1618 ), #9469, .T. ) ;
#921 = CARTESIAN_POINT ( 'NONE',  ( -3.187906586576829682, -9.105473976199601083, 1.812833570429532859 ) ) ;
#922 = DIRECTION ( 'NONE',  ( -0.000000000000000000, -0.000000000000000000, -1.000000000000000000 ) ) ;
#923 = CYLINDRICAL_SURFACE ( 'NONE', #19544, 2.500000000000000444 ) ;
#924 = VECTOR ( 'NONE', #1979, 1000.000000000000000 ) ;
#925 = LINE ( 'NONE', #827, #16027 ) ;
#926 = ADVANCED_FACE ( 'NONE', ( #14369 ), #17418, .T. ) ;
#927 = EDGE_CURVE ( 'NONE', #15982, #12948, #56, .T. ) ;
#928 = CARTESIAN_POINT ( 'NONE',  ( 10.65969141768317741, -22.98484643305507191, 0.9790045612916508100 ) ) ;
#929 = CARTESIAN_POINT ( 'NONE',  ( -13.12529397354238192, 5.014845663890295846, 4.833333333333344584 ) ) ;
#930 = VECTOR ( 'NONE', #4368, 1000.000000000000000 ) ;
#931 = CARTESIAN_POINT ( 'NONE',  ( -5.597191417683177406, -23.08622137881040359, 5.979004561291654696 ) ) ;
#932 = VERTEX_POINT ( 'NONE', #17729 ) ;
#933 = CARTESIAN_POINT ( 'NONE',  ( 10.74655858231679417, -21.94931252712234482, 5.250000000000000888 ) ) ;
#934 = CARTESIAN_POINT ( 'NONE',  ( -13.87500000000000178, 5.000000000000047962, 4.000000000000000000 ) ) ;
#935 = CARTESIAN_POINT ( 'NONE',  ( -13.43273460392801155, -18.08440250163749496, 6.268067769197452677 ) ) ;
#936 = EDGE_CURVE ( 'NONE', #17, #20705, #15840, .T. ) ;
#937 = CARTESIAN_POINT ( 'NONE',  ( 12.62155858231679417, -23.74999999999999645, 3.550687472877651629 ) ) ;
#938 = LINE ( 'NONE', #739, #9319 ) ;
#939 = EDGE_LOOP ( 'NONE', ( #171, #11278, #1339, #9867 ) ) ;
#940 = ORIENTED_EDGE ( 'NONE', *, *, #4469, .F. ) ;
#941 = CARTESIAN_POINT ( 'NONE',  ( 13.81626551376501588, 2.033908445126689557, 5.950679699622869911 ) ) ;
#942 = DIRECTION ( 'NONE',  ( -0.000000000000000000, -0.000000000000000000, -1.000000000000000000 ) ) ;
#943 = ORIENTED_EDGE ( 'NONE', *, *, #17591, .T. ) ;
#944 = AXIS2_PLACEMENT_3D ( 'NONE', #2419, #18922, #9187 ) ;
#945 = CARTESIAN_POINT ( 'NONE',  ( 9.555650798910054533, 0.000000000000000000, 1.000000000000000000 ) ) ;
#946 = DIRECTION ( 'NONE',  ( -0.000000000000000000, -0.000000000000000000, -1.000000000000000000 ) ) ;
#947 = CARTESIAN_POINT ( 'NONE',  ( -11.59030858231679417, -21.32581373872472597, 1.729004561291657582 ) ) ;
#948 = CARTESIAN_POINT ( 'NONE',  ( 11.00000000000000000, -20.29006350946107418, 5.466506350946110260 ) ) ;
#949 = EDGE_CURVE ( 'NONE', #20101, #8920, #1728, .T. ) ;
#950 = LINE ( 'NONE', #5663, #9851 ) ;
#951 = CARTESIAN_POINT ( 'NONE',  ( 3.002445346198714837, -11.66215945560911749, 2.276826493710632171 ) ) ;
#952 = CARTESIAN_POINT ( 'NONE',  ( 27.94203811574922725, 3.231447299068595019E-14, 0.000000000000000000 ) ) ;
#953 = CARTESIAN_POINT ( 'NONE',  ( -13.37499999999998224, -19.49999999999998934, 4.166666666666637653 ) ) ;
#954 = CARTESIAN_POINT ( 'NONE',  ( 9.555650798910054533, 9.000000000000001776, 1.000000000000000000 ) ) ;
#955 = CARTESIAN_POINT ( 'NONE',  ( -13.37499999999998401, -20.99999999999998934, 2.439580858552613751 ) ) ;
#956 = AXIS2_PLACEMENT_3D ( 'NONE', #10190, #19720, #5172 ) ;
#957 = CARTESIAN_POINT ( 'NONE',  ( -11.00000000000000000, -19.49999999999999645, 5.000000000000000000 ) ) ;
#958 = CARTESIAN_POINT ( 'NONE',  ( 5.684058582316795949, -21.32873467460644079, 2.757051763020455404 ) ) ;
#959 = EDGE_CURVE ( 'NONE', #17043, #11462, #15938, .T. ) ;
#960 = CARTESIAN_POINT ( 'NONE',  ( 11.97219141768317918, -22.97900456129165292, 3.035098964749240125 ) ) ;
#961 = CARTESIAN_POINT ( 'NONE',  ( -4.687312169500634340, -21.70215802671379990, 4.455959925339818106 ) ) ;
#962 = VERTEX_POINT ( 'NONE', #11238 ) ;
#963 = CARTESIAN_POINT ( 'NONE',  ( 13.09106898171683930, 4.036483576700608644, 5.256123545019964816 ) ) ;
#964 = CARTESIAN_POINT ( 'NONE',  ( 4.750698171653723989, 16.00000000000000000, 1.000000000000000000 ) ) ;
#965 = VERTEX_POINT ( 'NONE', #20572 ) ;
#966 = ORIENTED_EDGE ( 'NONE', *, *, #1652, .F. ) ;
#967 = FACE_OUTER_BOUND ( 'NONE', #17994, .T. ) ;
#968 = VECTOR ( 'NONE', #2534, 1000.000000000000000 ) ;
#969 = DIRECTION ( 'NONE',  ( 1.000000000000000000, 0.000000000000000000, -0.000000000000000000 ) ) ;
#970 = EDGE_CURVE ( 'NONE', #122, #20224, #19412, .T. ) ;
#971 = VECTOR ( 'NONE', #5445, 1000.000000000000000 ) ;
#972 = EDGE_CURVE ( 'NONE', #9402, #17667, #9669, .T. ) ;
#973 = VECTOR ( 'NONE', #693, 1000.000000000000000 ) ;
#974 = CARTESIAN_POINT ( 'NONE',  ( -2.875042468481914248, -11.91375063635796039, 3.091440134965714126 ) ) ;
#975 = CARTESIAN_POINT ( 'NONE',  ( -13.84504075139246915, 3.487057945321567765, 5.981929699623240282 ) ) ;
#976 = CARTESIAN_POINT ( 'NONE',  ( 10.18924542913430820, 10.00000000000000000, 1.000000000000000000 ) ) ;
#977 = CARTESIAN_POINT ( 'NONE',  ( 1.513434189748285918, -9.864917468222230923, 2.372643865078341019 ) ) ;
#978 = DIRECTION ( 'NONE',  ( 0.000000000000000000, 1.000000000000000000, 0.000000000000000000 ) ) ;
#979 = CARTESIAN_POINT ( 'NONE',  ( 11.00000000000000000, -18.49999999999999645, 4.000000000000000000 ) ) ;
#980 = LINE ( 'NONE', #17184, #6298 ) ;
#981 = CARTESIAN_POINT ( 'NONE',  ( -8.777808582316797725, -19.52099543870833642, 2.413778621189609286 ) ) ;
#982 = CARTESIAN_POINT ( 'NONE',  ( -2.512468814886674284, -13.43512376012158782, 2.539544162874482591 ) ) ;
#983 = AXIS2_PLACEMENT_3D ( 'NONE', #16894, #20474, #12499 ) ;
#984 = ORIENTED_EDGE ( 'NONE', *, *, #7515, .F. ) ;
#985 = CARTESIAN_POINT ( 'NONE',  ( -13.37499999999998224, -19.49999999999998934, 4.291666666666699825 ) ) ;
#986 = CARTESIAN_POINT ( 'NONE',  ( -1.437849085826860884, 11.64110105645932691, 0.000000000000000000 ) ) ;
#987 = ADVANCED_FACE ( 'NONE', ( #3397 ), #11143, .F. ) ;
#988 = CARTESIAN_POINT ( 'NONE',  ( 10.09719141768317741, -23.08622137881040359, 5.979004561291654696 ) ) ;
#989 = CARTESIAN_POINT ( 'NONE',  ( -10.56594141768317741, -22.67126532539353789, 2.757051763020445634 ) ) ;
#990 = AXIS2_PLACEMENT_3D ( 'NONE', #20222, #5883, #4722 ) ;
#991 = ORIENTED_EDGE ( 'NONE', *, *, #5535, .F. ) ;
#992 = CARTESIAN_POINT ( 'NONE',  ( 13.40022353639839103, -18.97621141187856608, 5.498856782956575984 ) ) ;
#993 = DIRECTION ( 'NONE',  ( -1.000000000000000000, -0.000000000000000000, -0.000000000000000000 ) ) ;
#994 = ORIENTED_EDGE ( 'NONE', *, *, #11563, .T. ) ;
#995 = VERTEX_POINT ( 'NONE', #20668 ) ;
#996 = LINE ( 'NONE', #20151, #19846 ) ;
#997 = EDGE_LOOP ( 'NONE', ( #14226, #5207, #13822, #2454 ) ) ;
#998 = CARTESIAN_POINT ( 'NONE',  ( -13.84983662433050178, 3.729249528687784920, 5.987138032956566214 ) ) ;
#999 = VERTEX_POINT ( 'NONE', #14478 ) ;
#1000 = CARTESIAN_POINT ( 'NONE',  ( 25.37918902992234393, 0.000000000000000000, 1.000000000000000000 ) ) ;
#1001 = LINE ( 'NONE', #7082, #16680 ) ;
#1002 =( GEOMETRIC_REPRESENTATION_CONTEXT ( 3 ) GLOBAL_UNCERTAINTY_ASSIGNED_CONTEXT ( ( #2948 ) ) GLOBAL_UNIT_ASSIGNED_CONTEXT ( ( #5234, #16426, #16621 ) ) REPRESENTATION_CONTEXT ( 'NONE', 'WORKASPACE' ) );
#1003 = CARTESIAN_POINT ( 'NONE',  ( 23.31633994409548549, 0.000000000000000000, 1.000000000000000000 ) ) ;
#1004 = CARTESIAN_POINT ( 'NONE',  ( 2.445888733774860935, -8.532121313016713060, 2.415585152653916712 ) ) ;
#1005 = LINE ( 'NONE', #7699, #8827 ) ;
#1006 = AXIS2_PLACEMENT_3D ( 'NONE', #15854, #3208, #9485 ) ;
#1007 = VECTOR ( 'NONE', #12119, 1000.000000000000000 ) ;
#1008 = CARTESIAN_POINT ( 'NONE',  ( 12.62499999999998401, -20.99999999999998934, 2.439580858552613751 ) ) ;
#1009 = CARTESIAN_POINT ( 'NONE',  ( 7.499999999999999112, -24.49999999999999289, 4.000000000000000000 ) ) ;
#1010 = DIRECTION ( 'NONE',  ( -1.000000000000000000, -1.192622389734054877E-16, 0.000000000000000000 ) ) ;
#1011 = CARTESIAN_POINT ( 'NONE',  ( 13.12529397354238192, 5.014845663890295846, 4.791666666666685614 ) ) ;
#1012 = CARTESIAN_POINT ( 'NONE',  ( 11.87844141768317741, -22.99999999999999645, 3.449312527122335048 ) ) ;
#1013 = CARTESIAN_POINT ( 'NONE',  ( -12.62562019941893432, -20.21867992933967173, 4.757612834768309540 ) ) ;
#1014 = CARTESIAN_POINT ( 'NONE',  ( -11.68405858231679595, -21.32873467460644079, 2.757051763020455404 ) ) ;
#1015 = ADVANCED_FACE ( 'NONE', ( #8213 ), #4758, .T. ) ;
#1016 = CARTESIAN_POINT ( 'NONE',  ( -10.84719141768317741, -20.91377862118959285, 1.020995438708345082 ) ) ;
#1017 = EDGE_LOOP ( 'NONE', ( #9052, #2300, #4060, #7390 ) ) ;
#1018 = CARTESIAN_POINT ( 'NONE',  ( 12.65396917024039958, -18.03705690286155772, 4.783553440007634272 ) ) ;
#1019 = CARTESIAN_POINT ( 'NONE',  ( -13.12529418130016445, 5.014856155665242454, 4.958178834604180629 ) ) ;
#1020 = VECTOR ( 'NONE', #18657, 1000.000000000000000 ) ;
#1021 = VECTOR ( 'NONE', #20699, 1000.000000000000000 ) ;
#1022 = ORIENTED_EDGE ( 'NONE', *, *, #10245, .T. ) ;
#1023 = CARTESIAN_POINT ( 'NONE',  ( -15.00000000000000000, -6.000000000000000000, 2.000000000000000000 ) ) ;
#1024 = FACE_OUTER_BOUND ( 'NONE', #15421, .T. ) ;
#1025 = ORIENTED_EDGE ( 'NONE', *, *, #18401, .F. ) ;
#1026 = CARTESIAN_POINT ( 'NONE',  ( 2.203959450683124377, -9.262433282444222371, 2.410528873095051594 ) ) ;
#1027 = ORIENTED_EDGE ( 'NONE', *, *, #17853, .T. ) ;
#1028 = VECTOR ( 'NONE', #4358, 1000.000000000000000 ) ;
#1029 = VECTOR ( 'NONE', #5552, 1000.000000000000000 ) ;
#1030 = EDGE_CURVE ( 'NONE', #9195, #15413, #4961, .T. ) ;
#1031 = ORIENTED_EDGE ( 'NONE', *, *, #1736, .T. ) ;
#1032 = DIRECTION ( 'NONE',  ( 1.000000000000000000, 0.000000000000000000, -0.000000000000000000 ) ) ;
#1033 = CARTESIAN_POINT ( 'NONE',  ( -0.000000000000000000, 10.00000000000000000, 0.000000000000000000 ) ) ;
#1034 = CARTESIAN_POINT ( 'NONE',  ( -1.711347482507859397, -9.865394108634699677, 1.622766275858107621 ) ) ;
#1035 = PLANE ( 'NONE',  #7985 ) ;
#1036 = FACE_OUTER_BOUND ( 'NONE', #17096, .T. ) ;
#1037 = CARTESIAN_POINT ( 'NONE',  ( 3.747260319564023501, 0.000000000000000000, 0.000000000000000000 ) ) ;
#1038 = CARTESIAN_POINT ( 'NONE',  ( 11.40969141768317918, -21.01515356694492098, 6.020995438708349745 ) ) ;
#1039 = CARTESIAN_POINT ( 'NONE',  ( -13.06655316810189227, 2.048434989138931961, 5.965524842914772030 ) ) ;
#1040 = VECTOR ( 'NONE', #11032, 1000.000000000000000 ) ;
#1041 = CARTESIAN_POINT ( 'NONE',  ( -3.974842109207560537, -21.73478823434188456, 6.006404853634143670 ) ) ;
#1042 = VECTOR ( 'NONE', #2570, 1000.000000000000000 ) ;
#1043 = AXIS2_PLACEMENT_3D ( 'NONE', #17057, #2736, #9115 ) ;
#1044 = ORIENTED_EDGE ( 'NONE', *, *, #9355, .F. ) ;
#1045 = CARTESIAN_POINT ( 'NONE',  ( 10.37155858231679417, -20.24999999999999289, 3.449312527122348371 ) ) ;
#1046 = CARTESIAN_POINT ( 'NONE',  ( -5.381197846483055436, -14.00000000000000000, 2.000000000000000000 ) ) ;
#1047 = CARTESIAN_POINT ( 'NONE',  ( -13.48548920624593883, -15.42029508461213716, 6.325359435864005064 ) ) ;
#1048 = VECTOR ( 'NONE', #18245, 1000.000000000000000 ) ;
#1049 = EDGE_CURVE ( 'NONE', #9910, #11689, #11331, .T. ) ;
#1050 = CARTESIAN_POINT ( 'NONE',  ( 11.40280858231679417, -22.77556120703056308, 1.770995438708339975 ) ) ;
#1051 = CARTESIAN_POINT ( 'NONE',  ( 4.247260319564023945, 0.000000000000000000, 1.000000000000000000 ) ) ;
#1052 = ORIENTED_EDGE ( 'NONE', *, *, #10950, .F. ) ;
#1053 = ORIENTED_EDGE ( 'NONE', *, *, #3524, .T. ) ;
#1054 = CARTESIAN_POINT ( 'NONE',  ( 13.60059015675642513, -9.607697083824668027, 6.450359435862663027 ) ) ;
#1055 = CARTESIAN_POINT ( 'NONE',  ( -2.786182376113650605, -10.12667130264514626, 1.882483419865550900 ) ) ;
#1056 =( NAMED_UNIT ( * ) PLANE_ANGLE_UNIT ( ) SI_UNIT ( $, .RADIAN. ) );
#1057 = ORIENTED_EDGE ( 'NONE', *, *, #3262, .T. ) ;
#1058 = FACE_OUTER_BOUND ( 'NONE', #15885, .T. ) ;
#1059 = EDGE_CURVE ( 'NONE', #17561, #14618, #6947, .T. ) ;
#1060 = EDGE_CURVE ( 'NONE', #11555, #13250, #3497, .T. ) ;
#1061 = ORIENTED_EDGE ( 'NONE', *, *, #19045, .T. ) ;
#1062 = CARTESIAN_POINT ( 'NONE',  ( 18.44064177244175440, 10.00000000000000000, 1.000000000000000000 ) ) ;
#1063 = VECTOR ( 'NONE', #10481, 1000.000000000000000 ) ;
#1064 = CARTESIAN_POINT ( 'NONE',  ( -16.62779268661489951, 11.64110105645932691, 10.00000000000000000 ) ) ;
#1065 = CARTESIAN_POINT ( 'NONE',  ( 11.99178095869207006, 9.000000000000001776, 0.000000000000000000 ) ) ;
#1066 = CARTESIAN_POINT ( 'NONE',  ( 2.589709240944451096, -9.559844081062008669, 1.736909907557668165 ) ) ;
#1067 = LINE ( 'NONE', #9213, #14396 ) ;
#1068 = CARTESIAN_POINT ( 'NONE',  ( -13.09001666039658573, 3.983341349998239966, 5.257104358157307367 ) ) ;
#1069 = CARTESIAN_POINT ( 'NONE',  ( 10.27780858231679417, -20.27099543870833642, 2.724438792969431589 ) ) ;
#1070 = CARTESIAN_POINT ( 'NONE',  ( -13.37499999999998224, -20.99999999999991829, 4.333333333333343695 ) ) ;
#1071 = CARTESIAN_POINT ( 'NONE',  ( -1.561130159782011306, 9.000000000000001776, 1.000000000000000000 ) ) ;
#1072 = CARTESIAN_POINT ( 'NONE',  ( 10.18405858231679417, -20.79840458871652942, 2.226721677130544030 ) ) ;
#1073 = AXIS2_PLACEMENT_3D ( 'NONE', #16519, #16419, #13270 ) ;
#1074 = EDGE_CURVE ( 'NONE', #10713, #19625, #10285, .T. ) ;
#1075 = CARTESIAN_POINT ( 'NONE',  ( 11.12844141768317741, -20.99999999999999645, 3.550687472877664952 ) ) ;
#1076 = CARTESIAN_POINT ( 'NONE',  ( -12.05905858231679417, -20.72672167713054137, 4.701595411283463477 ) ) ;
#1077 = EDGE_LOOP ( 'NONE', ( #18859, #14241, #20611, #6809, #18260 ) ) ;
#1078 = CARTESIAN_POINT ( 'NONE',  ( 13.47561960997282071, -14.41870969638424071, 4.846833296715798767 ) ) ;
#1079 = CARTESIAN_POINT ( 'NONE',  ( -0.000000000000000000, 11.64110105645932691, 0.000000000000000000 ) ) ;
#1080 = ORIENTED_EDGE ( 'NONE', *, *, #1425, .F. ) ;
#1081 = UNCERTAINTY_MEASURE_WITH_UNIT (LENGTH_MEASURE( 1.000000000000000082E-05 ), #17353, 'distance_accuracy_value', 'NONE');
#1082 = ORIENTED_EDGE ( 'NONE', *, *, #7355, .F. ) ;
#1083 = DIRECTION ( 'NONE',  ( 0.000000000000000000, -1.000000000000000000, 0.000000000000000000 ) ) ;
#1084 = CARTESIAN_POINT ( 'NONE',  ( -12.62499979224180180, -20.25001049178813162, 4.458178821399696012 ) ) ;
#1085 = DIRECTION ( 'NONE',  ( 0.000000000000000000, 1.000000000000000000, -0.000000000000000000 ) ) ;
#1086 = CARTESIAN_POINT ( 'NONE',  ( -13.87367531042247748, 4.933103176334663331, 5.324010972534209074 ) ) ;
#1087 = ADVANCED_FACE ( 'NONE', ( #2230 ), #18348, .T. ) ;
#1088 = VECTOR ( 'NONE', #11873, 1000.000000000000000 ) ;
#1089 = DIRECTION ( 'NONE',  ( -1.000000000000000000, 0.000000000000000000, 0.000000000000000000 ) ) ;
#1090 = CARTESIAN_POINT ( 'NONE',  ( -12.62500000000001954, -20.25000000000274269, 4.083333333315724012 ) ) ;
#1091 = DIRECTION ( 'NONE',  ( 0.000000000000000000, 0.000000000000000000, 1.000000000000000000 ) ) ;
#1092 = FACE_OUTER_BOUND ( 'NONE', #7198, .T. ) ;
#1093 = CARTESIAN_POINT ( 'NONE',  ( -1.513434189748285696, -9.114917468222230923, 2.372643865078341019 ) ) ;
#1094 = CARTESIAN_POINT ( 'NONE',  ( -11.77780858231679595, -19.52099543870833642, 2.413778621189609286 ) ) ;
#1095 = CARTESIAN_POINT ( 'NONE',  ( -2.844469389063872811, -10.54053385813977606, 1.988770633557972012 ) ) ;
#1096 = ORIENTED_EDGE ( 'NONE', *, *, #15655, .F. ) ;
#1097 = CARTESIAN_POINT ( 'NONE',  ( -13.37500000000002132, -20.25000000000274269, 4.083333333315724012 ) ) ;
#1098 = CARTESIAN_POINT ( 'NONE',  ( -13.49999999999998401, -24.49999999999999289, 4.000000000000000000 ) ) ;
#1099 = EDGE_CURVE ( 'NONE', #2580, #20101, #18033, .T. ) ;
#1100 = CARTESIAN_POINT ( 'NONE',  ( 5.590308582316795949, -21.01515356694490322, 0.9790045612916562501 ) ) ;
#1101 = CARTESIAN_POINT ( 'NONE',  ( -7.659691417683177406, -22.36352608949543352, 2.479004561291652031 ) ) ;
#1102 = ORIENTED_EDGE ( 'NONE', *, *, #4112, .T. ) ;
#1103 = ADVANCED_FACE ( 'NONE', ( #10185 ), #2134, .T. ) ;
#1104 = CARTESIAN_POINT ( 'NONE',  ( 13.54769662923970763, -11.52882022337116119, 5.659013032956382361 ) ) ;
#1105 = DIRECTION ( 'NONE',  ( 1.000000000000000000, 0.000000000000000000, -0.000000000000000000 ) ) ;
#1106 = ORIENTED_EDGE ( 'NONE', *, *, #14014, .T. ) ;
#1107 = ORIENTED_EDGE ( 'NONE', *, *, #8472, .T. ) ;
#1108 = VECTOR ( 'NONE', #14446, 1000.000000000000000 ) ;
#1109 = DIRECTION ( 'NONE',  ( 0.000000000000000000, 1.000000000000000000, 0.000000000000000000 ) ) ;
#1110 = EDGE_CURVE ( 'NONE', #4929, #14114, #16258, .T. ) ;
#1111 = VERTEX_POINT ( 'NONE', #3595 ) ;
#1112 = CARTESIAN_POINT ( 'NONE',  ( -13.75871503850933841, -0.8723905552644914962, 5.888179699623941943 ) ) ;
#1113 = DIRECTION ( 'NONE',  ( 0.000000000000000000, -1.000000000000000000, 0.000000000000000000 ) ) ;
#1114 = ORIENTED_EDGE ( 'NONE', *, *, #4469, .T. ) ;
#1115 = CARTESIAN_POINT ( 'NONE',  ( -22.85856191738413656, 4.999999999999999112, 1.000000000000000000 ) ) ;
#1116 = EDGE_CURVE ( 'NONE', #2917, #8843, #13323, .T. ) ;
#1117 = LINE ( 'NONE', #18579, #5327 ) ;
#1118 = DIRECTION ( 'NONE',  ( -1.000000000000000000, 0.000000000000000000, 0.000000000000000000 ) ) ;
#1119 = CARTESIAN_POINT ( 'NONE',  ( 2.830107938415192148, -10.43856789473369950, 1.962583737180462418 ) ) ;
#1120 = CARTESIAN_POINT ( 'NONE',  ( -14.49999999999998579, -18.49999999999999645, 4.000000000000000000 ) ) ;
#1121 = CARTESIAN_POINT ( 'NONE',  ( -0.000000000000000000, 10.00000000000000000, 0.000000000000000000 ) ) ;
#1122 = AXIS2_PLACEMENT_3D ( 'NONE', #3753, #9921, #5424 ) ;
#1123 = CARTESIAN_POINT ( 'NONE',  ( -30.80549002841696193, 5.431839045955507927, 1.000000000000000000 ) ) ;
#1124 = PLANE ( 'NONE',  #12366 ) ;
#1125 = LINE ( 'NONE', #17006, #6012 ) ;
#1126 = CARTESIAN_POINT ( 'NONE',  ( 8.128441417683177406, -20.99999999999999645, 3.550687472877664952 ) ) ;
#1127 = CARTESIAN_POINT ( 'NONE',  ( -13.09532840572934376, 3.501584489333809724, 5.996774842915142401 ) ) ;
#1128 = CARTESIAN_POINT ( 'NONE',  ( -8.871558582316795949, -20.99999999999999645, 3.449312527122348371 ) ) ;
#1129 = CARTESIAN_POINT ( 'NONE',  ( -7.753441417683177406, -21.94931252712233061, 0.9999999999999978906 ) ) ;
#1130 = EDGE_LOOP ( 'NONE', ( #10669, #9207, #839, #8430 ) ) ;
#1131 = CARTESIAN_POINT ( 'NONE',  ( 12.62506359033936754, -19.49678868786235597, 4.541393094775662220 ) ) ;
#1132 = CARTESIAN_POINT ( 'NONE',  ( -12.83635126708105823, -9.576761012430582198, 5.715524842913705328 ) ) ;
#1133 = ORIENTED_EDGE ( 'NONE', *, *, #10725, .T. ) ;
#1134 = FACE_OUTER_BOUND ( 'NONE', #3521, .T. ) ;
#1135 = ORIENTED_EDGE ( 'NONE', *, *, #13755, .F. ) ;
#1136 = CARTESIAN_POINT ( 'NONE',  ( 1.824218240560544047, -9.921717538097572842, 2.387231257717697286 ) ) ;
#1137 = VERTEX_POINT ( 'NONE', #1925 ) ;
#1138 = CARTESIAN_POINT ( 'NONE',  ( 18.44064177244175440, 0.000000000000000000, 1.000000000000000000 ) ) ;
#1139 = EDGE_CURVE ( 'NONE', #18061, #13178, #5166, .T. ) ;
#1140 = LINE ( 'NONE', #1033, #20003 ) ;
#1141 = CARTESIAN_POINT ( 'NONE',  ( -2.049450250860079592, -10.15122911285664564, 1.696174415070213382 ) ) ;
#1142 = CARTESIAN_POINT ( 'NONE',  ( -5.999999999999999112, -7.500000000000047073, 9.999999999999998224 ) ) ;
#1143 = LINE ( 'NONE', #10551, #6290 ) ;
#1144 = CARTESIAN_POINT ( 'NONE',  ( 25.37918902992234393, 10.00000000000000000, 0.000000000000000000 ) ) ;
#1145 = VECTOR ( 'NONE', #205, 1000.000000000000000 ) ;
#1146 = CARTESIAN_POINT ( 'NONE',  ( 10.75344141768317741, -21.94931252712233061, 0.9999999999999978906 ) ) ;
#1147 = CARTESIAN_POINT ( 'NONE',  ( -13.12119116326504908, 4.807653744879115010, 5.626470997801169105 ) ) ;
#1148 = CARTESIAN_POINT ( 'NONE',  ( -10.65969141768318096, -22.67418626127524917, 1.729004561291651809 ) ) ;
#1149 = VERTEX_POINT ( 'NONE', #11547 ) ;
#1150 = CARTESIAN_POINT ( 'NONE',  ( 11.02780858231679595, -23.72900456129165647, 4.275561207030568411 ) ) ;
#1151 = CARTESIAN_POINT ( 'NONE',  ( -9.999999999999998224, -30.00000000000000355, 1.000000000000000000 ) ) ;
#1152 = CARTESIAN_POINT ( 'NONE',  ( -13.87144757537903494, 4.070602556641903291, 6.741633940066556363 ) ) ;
#1153 = CARTESIAN_POINT ( 'NONE',  ( 11.02780858231679595, -23.72900456129165647, 4.275561207030568411 ) ) ;
#1154 = FACE_OUTER_BOUND ( 'NONE', #17723, .T. ) ;
#1155 = ORIENTED_EDGE ( 'NONE', *, *, #14762, .T. ) ;
#1156 = ORIENTED_EDGE ( 'NONE', *, *, #3778, .T. ) ;
#1157 = CARTESIAN_POINT ( 'NONE',  ( 13.44712222274167246, -17.35782775154002522, 6.283692769197384287 ) ) ;
#1158 = CARTESIAN_POINT ( 'NONE',  ( -3.499999999999997780, -24.49999999999999289, 4.000000000000000000 ) ) ;
#1159 = ORIENTED_EDGE ( 'NONE', *, *, #7829, .F. ) ;
#1160 = DIRECTION ( 'NONE',  ( 1.000000000000000000, -0.000000000000000000, -0.000000000000000000 ) ) ;
#1161 = ORIENTED_EDGE ( 'NONE', *, *, #12049, .F. ) ;
#1162 = CARTESIAN_POINT ( 'NONE',  ( 13.49999999999998401, -21.99999999999999645, 11.68378559369222280 ) ) ;
#1163 = CARTESIAN_POINT ( 'NONE',  ( 13.87470602645761986, 4.985154336109792972, 4.916666666666650087 ) ) ;
#1164 = CARTESIAN_POINT ( 'NONE',  ( 0.000000000000000000, 0.000000000000000000, 1.000000000000000000 ) ) ;
#1165 = CARTESIAN_POINT ( 'NONE',  ( 2.532303758294933704, -8.551221675625164664, 1.670490507339845054 ) ) ;
#1166 = EDGE_CURVE ( 'NONE', #9041, #10510, #13117, .T. ) ;
#1167 = DIRECTION ( 'NONE',  ( 1.156482317317871133E-15, -1.000000000000000000, 0.000000000000000000 ) ) ;
#1168 = CARTESIAN_POINT ( 'NONE',  ( -13.37499999999998224, -19.50000000000006040, 4.416666666666682062 ) ) ;
#1169 = LINE ( 'NONE', #856, #1063 ) ;
#1170 = CARTESIAN_POINT ( 'NONE',  ( -13.37543017851028893, -20.97827598523083026, 4.780017688621249761 ) ) ;
#1171 = CARTESIAN_POINT ( 'NONE',  ( 19.23630159782011617, 4.999999999999999112, 1.000000000000000000 ) ) ;
#1172 = EDGE_CURVE ( 'NONE', #20035, #2663, #3906, .T. ) ;
#1173 = CARTESIAN_POINT ( 'NONE',  ( 11.96530858231679595, -20.22900456129164937, 4.174186261275266929 ) ) ;
#1174 = EDGE_CURVE ( 'NONE', #8843, #4699, #14987, .T. ) ;
#1175 = CARTESIAN_POINT ( 'NONE',  ( 11.31594141768317741, -21.32873467460645145, 4.242948236979555254 ) ) ;
#1176 = CARTESIAN_POINT ( 'NONE',  ( -7.090308582316794173, -21.32581373872472597, 1.729004561291657582 ) ) ;
#1177 = ORIENTED_EDGE ( 'NONE', *, *, #15399, .T. ) ;
#1178 = CARTESIAN_POINT ( 'NONE',  ( 13.38090111944825367, -19.20199346786276351, 4.743968713382380464 ) ) ;
#1179 = FACE_OUTER_BOUND ( 'NONE', #10750, .T. ) ;
#1180 = VERTEX_POINT ( 'NONE', #19610 ) ;
#1181 = ORIENTED_EDGE ( 'NONE', *, *, #2244, .T. ) ;
#1182 = CARTESIAN_POINT ( 'NONE',  ( 6.183390479346035917, 9.000000000000001776, 0.000000000000000000 ) ) ;
#1183 = CARTESIAN_POINT ( 'NONE',  ( -12.64931222250080545, -19.02223276370786209, 5.512399842915133519 ) ) ;
#1184 = VECTOR ( 'NONE', #2415, 1000.000000000000000 ) ;
#1185 = VECTOR ( 'NONE', #17236, 1000.000000000000000 ) ;
#1186 = CARTESIAN_POINT ( 'NONE',  ( -13.86106797245302147, 4.296432608878145487, 5.947261916831099171 ) ) ;
#1187 = EDGE_CURVE ( 'NONE', #11689, #18614, #8308, .T. ) ;
#1188 = DIRECTION ( 'NONE',  ( 0.000000000000000000, 0.000000000000000000, 1.000000000000000000 ) ) ;
#1189 = CARTESIAN_POINT ( 'NONE',  ( 2.693754455098655409, -10.14181605509423711, 1.874202551270839123 ) ) ;
#1190 = PLANE ( 'NONE',  #11495 ) ;
#1191 = CARTESIAN_POINT ( 'NONE',  ( -14.49999999999998579, -25.49999999999999645, 4.000000000000000000 ) ) ;
#1192 = LINE ( 'NONE', #9038, #12638 ) ;
#1193 = CARTESIAN_POINT ( 'NONE',  ( -8.027808582316795949, -24.47900456129166358, 4.586221378810390270 ) ) ;
#1194 = CARTESIAN_POINT ( 'NONE',  ( -0.2815691515810352930, -9.114917468222230923, 1.622643865078524206 ) ) ;
#1195 = EDGE_CURVE ( 'NONE', #18185, #20045, #9975, .T. ) ;
#1196 = EDGE_LOOP ( 'NONE', ( #1515, #11815, #721, #16544 ) ) ;
#1197 = ADVANCED_FACE ( 'NONE', ( #5478 ), #562, .T. ) ;
#1198 = CARTESIAN_POINT ( 'NONE',  ( -13.84495141469777479, 4.232546442235974204, 5.040078719623224401 ) ) ;
#1199 = LINE ( 'NONE', #4441, #1374 ) ;
#1201 = CARTESIAN_POINT ( 'NONE',  ( 5.965308582316795949, -19.47900456129164937, 4.484846433055089676 ) ) ;
#1200 = APPLICATION_CONTEXT ( 'automotive_design' ) ;
#1202 = CARTESIAN_POINT ( 'NONE',  ( -4.659691417683177406, -22.36352608949543352, 2.479004561291652031 ) ) ;
#1203 = ORIENTED_EDGE ( 'NONE', *, *, #15128, .F. ) ;
#1204 = CARTESIAN_POINT ( 'NONE',  ( 13.87470602645415063, 4.985154336109792972, 3.333333333332063830 ) ) ;
#1205 = DIRECTION ( 'NONE',  ( -0.000000000000000000, 0.1264857625231113059, -0.9919684228235025047 ) ) ;
#1206 = ORIENTED_EDGE ( 'NONE', *, *, #9633, .F. ) ;
#1207 = EDGE_CURVE ( 'NONE', #1851, #19958, #13522, .T. ) ;
#1208 = ORIENTED_EDGE ( 'NONE', *, *, #4382, .T. ) ;
#1209 = LINE ( 'NONE', #13947, #18796 ) ;
#1210 = EDGE_LOOP ( 'NONE', ( #3460, #4701, #11385, #3949 ) ) ;
#1211 = CARTESIAN_POINT ( 'NONE',  ( -13.85343352903393388, 3.910893216212274925, 5.991044282956552891 ) ) ;
#1212 = CARTESIAN_POINT ( 'NONE',  ( 13.49999999999998401, -19.52007894294123957, 12.00000000000000000 ) ) ;
#1213 = VERTEX_POINT ( 'NONE', #11750 ) ;
#1214 = CARTESIAN_POINT ( 'NONE',  ( -14.49999999999998579, -18.49999999999999645, 1.000000000000000000 ) ) ;
#1215 = LINE ( 'NONE', #19203, #3009 ) ;
#1216 = EDGE_CURVE ( 'NONE', #11536, #7438, #16444, .T. ) ;
#1217 = LINE ( 'NONE', #13958, #17678 ) ;
#1218 = CARTESIAN_POINT ( 'NONE',  ( 3.342893013439646843, -9.383962644129466568, 1.884355023724047173 ) ) ;
#1219 = DIRECTION ( 'NONE',  ( -1.000000000000000000, 2.312964634635752916E-15, 0.000000000000000000 ) ) ;
#1220 = LINE ( 'NONE', #7595, #4069 ) ;
#1221 = DIRECTION ( 'NONE',  ( 0.000000000000000000, -0.000000000000000000, 1.000000000000000000 ) ) ;
#1222 = DIRECTION ( 'NONE',  ( -0.000000000000000000, -0.000000000000000000, -1.000000000000000000 ) ) ;
#1223 = DIRECTION ( 'NONE',  ( -0.000000000000000000, -0.000000000000000000, -1.000000000000000000 ) ) ;
#1224 = CARTESIAN_POINT ( 'NONE',  ( 7.378441417683177406, -22.99999999999999645, 3.449312527122335048 ) ) ;
#1225 = CARTESIAN_POINT ( 'NONE',  ( -13.12512971825177033, 5.006550771716304915, 5.133277049491872468 ) ) ;
#1226 = CARTESIAN_POINT ( 'NONE',  ( -9.246558582316795949, -21.94931252712234127, 4.499999999999999112 ) ) ;
#1227 = CARTESIAN_POINT ( 'NONE',  ( -10.37844141768317741, -24.50000000000000000, 3.449312527122335048 ) ) ;
#1228 = EDGE_LOOP ( 'NONE', ( #5307, #10202, #12279, #10206 ) ) ;
#1229 = CARTESIAN_POINT ( 'NONE',  ( 13.37499999999998224, -19.49999999999991473, 4.333333333333343695 ) ) ;
#1230 = CARTESIAN_POINT ( 'NONE',  ( -15.00000000000000000, -6.000000000000000000, 2.000000000000000000 ) ) ;
#1231 = VERTEX_POINT ( 'NONE', #2334 ) ;
#1232 = LINE ( 'NONE', #7714, #19995 ) ;
#1233 = ORIENTED_EDGE ( 'NONE', *, *, #720, .F. ) ;
#1234 = CARTESIAN_POINT ( 'NONE',  ( 1.904508877737772998, -9.138371295333994837, 2.378667276417936627 ) ) ;
#1235 = VECTOR ( 'NONE', #15090, 1000.000000000000000 ) ;
#1236 = ORIENTED_EDGE ( 'NONE', *, *, #17024, .T. ) ;
#1237 = DIRECTION ( 'NONE',  ( -0.000000000000000000, 0.000000000000000000, 1.000000000000000000 ) ) ;
#1238 = CARTESIAN_POINT ( 'NONE',  ( -10.43924542913431175, 0.000000000000000000, 1.000000000000000000 ) ) ;
#1239 = EDGE_CURVE ( 'NONE', #19704, #9634, #8725, .T. ) ;
#1240 = ADVANCED_FACE ( 'NONE', ( #11951 ), #5996, .T. ) ;
#1241 = CARTESIAN_POINT ( 'NONE',  ( -2.167793999318431197, -10.98794063836983703, 1.911058649813994315 ) ) ;
#1242 = CARTESIAN_POINT ( 'NONE',  ( -24.12918902992234393, 10.00000000000000000, 0.000000000000000000 ) ) ;
#1243 = CARTESIAN_POINT ( 'NONE',  ( 13.49999999999998401, -24.47992105705875332, 12.00000000000000000 ) ) ;
#1244 = CARTESIAN_POINT ( 'NONE',  ( 5.000000000000000000, -12.50000000000000000, 4.500000000000000888 ) ) ;
#1245 = AXIS2_PLACEMENT_3D ( 'NONE', #6195, #6294, #8185 ) ;
#1246 = CARTESIAN_POINT ( 'NONE',  ( 5.690941417683177406, -23.80360840875937001, 5.231925497173365081 ) ) ;
#1247 = SURFACE_STYLE_USAGE ( .BOTH. , #7732 ) ;
#1248 = CARTESIAN_POINT ( 'NONE',  ( -11.78469141768317563, -23.77099543870834353, 4.174186261275252718 ) ) ;
#1249 = ORIENTED_EDGE ( 'NONE', *, *, #3446, .F. ) ;
#1250 = CARTESIAN_POINT ( 'NONE',  ( 9.527808582316792396, -23.72900456129165647, 4.275561207030568411 ) ) ;
#1251 = LINE ( 'NONE', #7738, #13752 ) ;
#1252 = CARTESIAN_POINT ( 'NONE',  ( -13.40787921250184311, -19.33959976865745389, 6.241060671539915283 ) ) ;
#1253 = EDGE_CURVE ( 'NONE', #8718, #122, #12062, .T. ) ;
#1254 = CARTESIAN_POINT ( 'NONE',  ( 5.965308582316795949, -20.97900456129165647, 3.863526089495444626 ) ) ;
#1255 = DIRECTION ( 'NONE',  ( -3.469446951953611033E-15, -1.000000000000000000, 0.000000000000000000 ) ) ;
#1256 = EDGE_LOOP ( 'NONE', ( #18237, #3582, #15612, #20012 ) ) ;
#1257 = ORIENTED_EDGE ( 'NONE', *, *, #16437, .T. ) ;
#1258 = CARTESIAN_POINT ( 'NONE',  ( 13.40653076352726103, -19.40769644187082932, 6.236886054669082746 ) ) ;
#1259 = DIRECTION ( 'NONE',  ( 1.000000000000000000, 1.013672804646636068E-16, 0.000000000000000000 ) ) ;
#1260 = FILL_AREA_STYLE ('',( #15784 ) ) ;
#1261 = ORIENTED_EDGE ( 'NONE', *, *, #17407, .T. ) ;
#1262 = DIRECTION ( 'NONE',  ( -0.000000000000000000, 0.000000000000000000, -1.000000000000000000 ) ) ;
#1263 = ORIENTED_EDGE ( 'NONE', *, *, #16479, .T. ) ;
#1264 = CARTESIAN_POINT ( 'NONE',  ( -9.996558582316794173, -22.05068747287764452, 1.749999999999998446 ) ) ;
#1265 = CARTESIAN_POINT ( 'NONE',  ( 13.87470602645761808, 4.985154336109792972, 4.000000000000000000 ) ) ;
#1266 = FACE_OUTER_BOUND ( 'NONE', #2611, .T. ) ;
#1267 = CARTESIAN_POINT ( 'NONE',  ( 1.619022621591187150, -9.114917468222230923, 1.622643865078341463 ) ) ;
#1268 = FACE_OUTER_BOUND ( 'NONE', #18251, .T. ) ;
#1269 = CARTESIAN_POINT ( 'NONE',  ( -13.37514942709654164, -19.49245393162283690, 4.562067678168288509 ) ) ;
#1270 = CARTESIAN_POINT ( 'NONE',  ( 7.184058582316794173, -20.79840458871652942, 2.226721677130544030 ) ) ;
#1271 = CARTESIAN_POINT ( 'NONE',  ( -12.62499999999998224, -20.99999999999998934, 4.291666666666699825 ) ) ;
#1272 = DIRECTION ( 'NONE',  ( 0.000000000000000000, -1.000000000000000000, 0.000000000000000000 ) ) ;
#1273 = CARTESIAN_POINT ( 'NONE',  ( 5.496558582316795949, -22.05068747287764452, 2.499999999999999112 ) ) ;
#1274 = CARTESIAN_POINT ( 'NONE',  ( 10.09719141768317741, -22.46490103525075810, 4.479004561291653808 ) ) ;
#1275 = CARTESIAN_POINT ( 'NONE',  ( -12.06594141768317563, -23.20159541128344927, 2.226721677130534705 ) ) ;
#1276 = ORIENTED_EDGE ( 'NONE', *, *, #16635, .F. ) ;
#1277 = CARTESIAN_POINT ( 'NONE',  ( 13.09556065010287362, 4.263312830196960057, 5.034075356110313315 ) ) ;
#1278 = CARTESIAN_POINT ( 'NONE',  ( -2.781778019848414552, -10.09537774617444938, 1.874445651118397560 ) ) ;
#1279 = ORIENTED_EDGE ( 'NONE', *, *, #936, .T. ) ;
#1280 = VECTOR ( 'NONE', #19650, 1000.000000000000000 ) ;
#1281 = EDGE_CURVE ( 'NONE', #3253, #12082, #13929, .T. ) ;
#1282 = UNCERTAINTY_MEASURE_WITH_UNIT (LENGTH_MEASURE( 1.000000000000000082E-05 ), #8702, 'distance_accuracy_value', 'NONE');
#1283 = VERTEX_POINT ( 'NONE', #976 ) ;
#1284 = DIRECTION ( 'NONE',  ( 3.469446951953611033E-15, 1.000000000000000000, 0.000000000000000000 ) ) ;
#1285 = CARTESIAN_POINT ( 'NONE',  ( -13.06655316810189227, 2.048434989138931961, 5.965524842914772030 ) ) ;
#1286 = CARTESIAN_POINT ( 'NONE',  ( -1.513434189748285918, -8.364917468222230923, 2.372643865078341019 ) ) ;
#1287 = CARTESIAN_POINT ( 'NONE',  ( -13.39107665282975645, -19.43812903209671461, 5.476542851584349947 ) ) ;
#1288 = CARTESIAN_POINT ( 'NONE',  ( 10.05565079891005631, 4.999999999999999112, 0.000000000000000000 ) ) ;
#1289 = CARTESIAN_POINT ( 'NONE',  ( -7.626396343307448866, 0.000000000000000000, 1.000000000000000000 ) ) ;
#1290 = CARTESIAN_POINT ( 'NONE',  ( 14.00000000000000000, 7.867487981852999499E-15, 2.000000000000000000 ) ) ;
#1291 = VECTOR ( 'NONE', #2912, 1000.000000000000000 ) ;
#1292 = LINE ( 'NONE', #7570, #4387 ) ;
#1293 = CARTESIAN_POINT ( 'NONE',  ( -13.37155858231679595, -19.49999999999998934, 3.449312527122348371 ) ) ;
#1294 = CARTESIAN_POINT ( 'NONE',  ( -1.548630333695928618, -8.364917468222230923, 1.622643865078341907 ) ) ;
#1295 = ORIENTED_EDGE ( 'NONE', *, *, #5909, .F. ) ;
#1296 = CARTESIAN_POINT ( 'NONE',  ( -13.39296152110871851, -19.34294318400601753, 5.489418334493660012 ) ) ;
#1297 = DIRECTION ( 'NONE',  ( -0.000000000000000000, -0.000000000000000000, -1.000000000000000000 ) ) ;
#1298 = CARTESIAN_POINT ( 'NONE',  ( 4.717959273841179524, -21.63341328858655999, 5.993595146365859883 ) ) ;
#1299 = CARTESIAN_POINT ( 'NONE',  ( -12.62155858231679417, -22.99999999999999645, 3.550687472877652073 ) ) ;
#1300 = VERTEX_POINT ( 'NONE', #10814 ) ;
#1301 = CARTESIAN_POINT ( 'NONE',  ( 13.38172782443493602, -20.66024486603417643, 5.557997437521964734 ) ) ;
#1302 = CARTESIAN_POINT ( 'NONE',  ( 12.62499999998404121, -20.24999999996810729, 2.793053905886972998 ) ) ;
#1303 = VECTOR ( 'NONE', #14815, 1000.000000000000000 ) ;
#1304 = ORIENTED_EDGE ( 'NONE', *, *, #16771, .F. ) ;
#1305 = VECTOR ( 'NONE', #15964, 1000.000000000000000 ) ;
#1306 = ORIENTED_EDGE ( 'NONE', *, *, #3962, .F. ) ;
#1307 = CYLINDRICAL_SURFACE ( 'NONE', #12478, 1.000000000000002665 ) ;
#1308 = EDGE_CURVE ( 'NONE', #16594, #7416, #10706, .T. ) ;
#1309 = VECTOR ( 'NONE', #3879, 1000.000000000000000 ) ;
#1310 = VERTEX_POINT ( 'NONE', #2758 ) ;
#1311 = CARTESIAN_POINT ( 'NONE',  ( -13.85723511636018301, 4.102873376188801657, 5.986996695041598926 ) ) ;
#1312 = CARTESIAN_POINT ( 'NONE',  ( 1.937849085826861328, 0.000000000000000000, 1.000000000000000000 ) ) ;
#1313 = EDGE_CURVE ( 'NONE', #19341, #3875, #3984, .T. ) ;
#1314 = EDGE_CURVE ( 'NONE', #18960, #13229, #314, .T. ) ;
#1315 = VERTEX_POINT ( 'NONE', #7668 ) ;
#1316 = CARTESIAN_POINT ( 'NONE',  ( -3.944195004867014909, -21.61378581760806128, 5.207602947182413011 ) ) ;
#1317 = CARTESIAN_POINT ( 'NONE',  ( 4.000698171653723101, 10.00000000000000000, 0.000000000000000000 ) ) ;
#1318 = DIRECTION ( 'NONE',  ( -0.000000000000000000, -0.000000000000000000, -1.000000000000000000 ) ) ;
#1319 = VECTOR ( 'NONE', #14885, 1000.000000000000114 ) ;
#1320 = CARTESIAN_POINT ( 'NONE',  ( 2.722060606927515725, -8.660968749821154944, 1.698675748411476283 ) ) ;
#1321 = DIRECTION ( 'NONE',  ( 1.000000000000000000, 0.000000000000000000, 0.000000000000000000 ) ) ;
#1322 = VECTOR ( 'NONE', #11570, 1000.000000000000000 ) ;
#1323 = DIRECTION ( 'NONE',  ( 0.000000000000000000, 0.000000000000000000, 1.000000000000000000 ) ) ;
#1324 = VECTOR ( 'NONE', #8795, 1000.000000000000000 ) ;
#1325 = CARTESIAN_POINT ( 'NONE',  ( 21.25349085826861995, 10.00000000000000000, 1.000000000000000000 ) ) ;
#1326 = CARTESIAN_POINT ( 'NONE',  ( -7.499999999999999112, -18.49999999999999645, 6.500000000000000888 ) ) ;
#1327 = DIRECTION ( 'NONE',  ( -1.000000000000000000, 0.000000000000000000, 0.000000000000000000 ) ) ;
#1328 = PRODUCT_DEFINITION_SHAPE ( 'NONE', 'NONE',  #13790 ) ;
#1329 = CARTESIAN_POINT ( 'NONE',  ( 6.253441417683175629, -21.94931252712233061, 2.499999999999999112 ) ) ;
#1330 = CARTESIAN_POINT ( 'NONE',  ( -13.12463908936614132, 4.981774012991869505, 5.264611377988129171 ) ) ;
#1331 = CARTESIAN_POINT ( 'NONE',  ( -11.87155858231679595, -20.99999999999999645, 3.449312527122348371 ) ) ;
#1332 = CARTESIAN_POINT ( 'NONE',  ( -11.50344141768317563, -22.05068747287765873, 5.250000000000000888 ) ) ;
#1333 = EDGE_LOOP ( 'NONE', ( #7064, #9377, #7104, #5763 ) ) ;
#1334 = CARTESIAN_POINT ( 'NONE',  ( 13.09560260347216953, 4.265431475339161338, 5.020858537328734883 ) ) ;
#1335 = DIRECTION ( 'NONE',  ( 1.000000000000000000, 0.000000000000000000, 0.000000000000000000 ) ) ;
#1336 = EDGE_LOOP ( 'NONE', ( #16230, #11844, #20016, #16927 ) ) ;
#1337 = CARTESIAN_POINT ( 'NONE',  ( -7.626396343307448866, 10.00000000000000000, 0.000000000000000000 ) ) ;
#1338 = EDGE_CURVE ( 'NONE', #10660, #19958, #5662, .T. ) ;
#1339 = ORIENTED_EDGE ( 'NONE', *, *, #3529, .F. ) ;
#1340 = CARTESIAN_POINT ( 'NONE',  ( 3.047379876266447685, -13.13734219723468755, 3.405682891496055742 ) ) ;
#1341 = VECTOR ( 'NONE', #9743, 1000.000000000000000 ) ;
#1342 = ORIENTED_EDGE ( 'NONE', *, *, #13749, .F. ) ;
#1343 = DIRECTION ( 'NONE',  ( 1.000000000000000000, 0.000000000000000000, 0.000000000000000000 ) ) ;
#1344 = FACE_OUTER_BOUND ( 'NONE', #5696, .T. ) ;
#1345 = VECTOR ( 'NONE', #17736, 1000.000000000000114 ) ;
#1346 = CARTESIAN_POINT ( 'NONE',  ( -1.872293763630120678, -10.04602735435188698, 2.419156501869924369 ) ) ;
#1347 = PLANE ( 'NONE',  #2016 ) ;
#1348 = DIRECTION ( 'NONE',  ( 0.000000000000000000, 1.000000000000000000, -0.000000000000000000 ) ) ;
#1349 = DIRECTION ( 'NONE',  ( 0.000000000000000000, 0.000000000000000000, 1.000000000000000000 ) ) ;
#1350 = CARTESIAN_POINT ( 'NONE',  ( 8.409691417683177406, -21.01515356694492098, 6.020995438708349745 ) ) ;
#1351 = DIRECTION ( 'NONE',  ( -0.000000000000000000, 0.000000000000000000, -1.000000000000000000 ) ) ;
#1352 = CARTESIAN_POINT ( 'NONE',  ( -8.784691417683177406, -23.77099543870834353, 4.174186261275252718 ) ) ;
#1353 = ORIENTED_EDGE ( 'NONE', *, *, #7385, .T. ) ;
#1354 = CARTESIAN_POINT ( 'NONE',  ( 9.434058582316794173, -23.20159541128345992, 4.773278322869455970 ) ) ;
#1355 = DIRECTION ( 'NONE',  ( -0.000000000000000000, -0.000000000000000000, -1.000000000000000000 ) ) ;
#1356 = CARTESIAN_POINT ( 'NONE',  ( -12.62500028073152869, -20.99998582305707728, 4.544498183892649479 ) ) ;
#1357 = ORIENTED_EDGE ( 'NONE', *, *, #81, .T. ) ;
#1358 = VECTOR ( 'NONE', #18316, 1000.000000000000000 ) ;
#1359 = CARTESIAN_POINT ( 'NONE',  ( 8.027808582316792396, -23.72900456129165647, 4.275561207030568411 ) ) ;
#1360 = EDGE_CURVE ( 'NONE', #5898, #18235, #5688, .T. ) ;
#1361 = FACE_OUTER_BOUND ( 'NONE', #2818, .T. ) ;
#1362 = EDGE_CURVE ( 'NONE', #8225, #1180, #13727, .T. ) ;
#1363 = VERTEX_POINT ( 'NONE', #7566 ) ;
#1364 = DIRECTION ( 'NONE',  ( 1.000000000000000000, 0.000000000000000000, 0.000000000000000000 ) ) ;
#1365 = ORIENTED_EDGE ( 'NONE', *, *, #8366, .F. ) ;
#1366 = EDGE_CURVE ( 'NONE', #18502, #13489, #4431, .T. ) ;
#1367 = CARTESIAN_POINT ( 'NONE',  ( 15.00000000000001421, -29.99999999999998579, 0.000000000000000000 ) ) ;
#1368 = VERTEX_POINT ( 'NONE', #16768 ) ;
#1369 = CARTESIAN_POINT ( 'NONE',  ( -9.152808582316794173, -21.22443879296942626, 5.229004561291659137 ) ) ;
#1370 = CARTESIAN_POINT ( 'NONE',  ( 12.62562019941893432, -20.21867992933967173, 4.757612834768309540 ) ) ;
#1371 = LINE ( 'NONE', #20620, #5508 ) ;
#1372 = CARTESIAN_POINT ( 'NONE',  ( 2.121089610268797276, -8.411987239090384705, 1.634732322550447758 ) ) ;
#1373 = EDGE_CURVE ( 'NONE', #17295, #15081, #2438, .T. ) ;
#1374 = VECTOR ( 'NONE', #12173, 1000.000000000000000 ) ;
#1375 = VECTOR ( 'NONE', #5558, 1000.000000000000000 ) ;
#1376 = DIRECTION ( 'NONE',  ( -1.000000000000000000, -0.000000000000000000, -0.000000000000000000 ) ) ;
#1377 = CARTESIAN_POINT ( 'NONE',  ( -13.09080647246885576, 4.023226859705822278, 5.257958009367514229 ) ) ;
#1378 = CARTESIAN_POINT ( 'NONE',  ( 9.152808582316794173, -21.22443879296942626, 5.229004561291659137 ) ) ;
#1379 = CARTESIAN_POINT ( 'NONE',  ( -13.90411326029870409, 5.720219645086723759, 5.230514352905474063 ) ) ;
#1380 = CARTESIAN_POINT ( 'NONE',  ( 3.944195004867014909, -21.61378581760806128, 5.207602947182413011 ) ) ;
#1381 = CARTESIAN_POINT ( 'NONE',  ( 8.684058582316794173, -20.79840458871652942, 2.226721677130544030 ) ) ;
#1382 = CARTESIAN_POINT ( 'NONE',  ( 12.80905858231679417, -22.74294823697954016, 2.828734674606448785 ) ) ;
#1383 = CARTESIAN_POINT ( 'NONE',  ( -5.777808582316794173, -20.27099543870833642, 2.724438792969431589 ) ) ;
#1384 = ORIENTED_EDGE ( 'NONE', *, *, #2193, .F. ) ;
#1385 = CARTESIAN_POINT ( 'NONE',  ( 13.45643611822145225, -15.38747602984844853, 4.825999963382285429 ) ) ;
#1386 = CARTESIAN_POINT ( 'NONE',  ( -2.195822829018478473, -9.226849102155203042, 1.651390144731336163 ) ) ;
#1387 = ORIENTED_EDGE ( 'NONE', *, *, #5301, .T. ) ;
#1388 = AXIS2_PLACEMENT_3D ( 'NONE', #14457, #15917, #6202 ) ;
#1389 = ORIENTED_EDGE ( 'NONE', *, *, #4000, .T. ) ;
#1390 = DIRECTION ( 'NONE',  ( 1.000000000000000000, 0.000000000000000000, -0.000000000000000000 ) ) ;
#1391 = DIRECTION ( 'NONE',  ( 0.000000000000000000, 0.000000000000000000, -1.000000000000000000 ) ) ;
#1392 = CARTESIAN_POINT ( 'NONE',  ( -0.2815691515810352930, -9.114917468222230923, 2.372643865078523984 ) ) ;
#1393 = CARTESIAN_POINT ( 'NONE',  ( -13.38238173943565990, -19.87722215849730034, 5.285856107751903288 ) ) ;
#1394 = EDGE_CURVE ( 'NONE', #5367, #10647, #4116, .T. ) ;
#1395 = CARTESIAN_POINT ( 'NONE',  ( -14.49999999999998579, -21.99999999999999645, 11.68378559369222280 ) ) ;
#1396 = LINE ( 'NONE', #4624, #11203 ) ;
#1397 = CARTESIAN_POINT ( 'NONE',  ( 10.65280858231679240, -21.22443879296942626, 5.229004561291660025 ) ) ;
#1398 = DIRECTION ( 'NONE',  ( 0.000000000000000000, -0.000000000000000000, 1.000000000000000000 ) ) ;
#1399 = CARTESIAN_POINT ( 'NONE',  ( 13.10985494974158705, 3.485174961951963191, 6.746454579156001330 ) ) ;
#1400 = VECTOR ( 'NONE', #15536, 1000.000000000000000 ) ;
#1401 = CARTESIAN_POINT ( 'NONE',  ( -12.25344141768317741, -21.94931252712233061, 0.9999999999999978906 ) ) ;
#1402 = CARTESIAN_POINT ( 'NONE',  ( -1.939860967060266672, -10.52577007527361808, 2.542364016426418516 ) ) ;
#1403 = EDGE_LOOP ( 'NONE', ( #8385, #4546, #1263, #5932 ) ) ;
#1404 = CARTESIAN_POINT ( 'NONE',  ( -13.84311479963346869, 4.139797381492562600, 5.195993353439945395 ) ) ;
#1405 = DIRECTION ( 'NONE',  ( 1.000000000000000000, 0.000000000000000000, -0.000000000000000000 ) ) ;
#1406 = CARTESIAN_POINT ( 'NONE',  ( 8.690941417683177406, -23.80360840875937001, 5.231925497173365081 ) ) ;
#1407 = CARTESIAN_POINT ( 'NONE',  ( -6.065941417683177406, -22.67126532539353789, 2.757051763020445634 ) ) ;
#1408 = EDGE_LOOP ( 'NONE', ( #15317, #16815, #12977, #18861, #4503, #15029 ) ) ;
#1409 = EDGE_CURVE ( 'NONE', #3062, #10193, #8830, .T. ) ;
#1410 = CARTESIAN_POINT ( 'NONE',  ( 13.37526900345969771, -20.98641532528209908, 4.724331462949078464 ) ) ;
#1411 = CARTESIAN_POINT ( 'NONE',  ( 12.62745083560477966, -20.12623280195927933, 5.001038150054709419 ) ) ;
#1412 = DIRECTION ( 'NONE',  ( -6.938893903907222067E-15, -1.000000000000000000, 0.000000000000000000 ) ) ;
#1413 = ORIENTED_EDGE ( 'NONE', *, *, #8902, .T. ) ;
#1414 = ORIENTED_EDGE ( 'NONE', *, *, #6972, .T. ) ;
#1415 = CARTESIAN_POINT ( 'NONE',  ( -13.87066368810231154, 4.781016249162736820, 5.617237349937618696 ) ) ;
#1416 = VECTOR ( 'NONE', #15941, 1000.000000000000000 ) ;
#1417 = CARTESIAN_POINT ( 'NONE',  ( -13.82942202582513325, -0.3863038687793825532, 0.9889833525439024609 ) ) ;
#1418 = CARTESIAN_POINT ( 'NONE',  ( 17.30017143803810242, 4.999999999999999112, 1.000000000000000000 ) ) ;
#1419 = CARTESIAN_POINT ( 'NONE',  ( 0.000000000000000000, 16.00000000000000000, 1.000000000000000000 ) ) ;
#1420 = LINE ( 'NONE', #7695, #9692 ) ;
#1421 = DIRECTION ( 'NONE',  ( 0.000000000000000000, -0.000000000000000000, 1.000000000000000000 ) ) ;
#1422 = CARTESIAN_POINT ( 'NONE',  ( 3.502569552650398155, -9.961070227720959736, 2.032567780072621400 ) ) ;
#1423 = CARTESIAN_POINT ( 'NONE',  ( 11.49178095869207006, 0.000000000000000000, 1.000000000000000000 ) ) ;
#1424 = CARTESIAN_POINT ( 'NONE',  ( -27.00000000000000000, 0.000000000000000000, 0.000000000000000000 ) ) ;
#1425 = EDGE_CURVE ( 'NONE', #10713, #6994, #6105, .T. ) ;
#1426 = CARTESIAN_POINT ( 'NONE',  ( 0.000000000000000000, 9.000000000000001776, 0.000000000000000000 ) ) ;
#1427 = LINE ( 'NONE', #10849, #1700 ) ;
#1428 = CARTESIAN_POINT ( 'NONE',  ( -13.33466323279248122, -20.44601834413422026, 3.454345736197117045 ) ) ;
#1429 = CARTESIAN_POINT ( 'NONE',  ( 7.565941417683177406, -22.67126532539353789, 2.757051763020445634 ) ) ;
#1430 = CARTESIAN_POINT ( 'NONE',  ( -12.91308523408712183, -5.701695678577235249, 5.798858176249892082 ) ) ;
#1431 = CARTESIAN_POINT ( 'NONE',  ( -7.559058582316795949, -21.25705176302045274, 4.171265325393551215 ) ) ;
#1432 = VECTOR ( 'NONE', #9969, 1000.000000000000000 ) ;
#1433 = CARTESIAN_POINT ( 'NONE',  ( -10.56594141768317741, -23.20159541128344927, 2.226721677130534705 ) ) ;
#1434 = VERTEX_POINT ( 'NONE', #18655 ) ;
#1435 = EDGE_CURVE ( 'NONE', #7660, #4902, #17180, .T. ) ;
#1436 = CARTESIAN_POINT ( 'NONE',  ( 13.37505992445764136, -19.49697381488866554, 4.539006848837218833 ) ) ;
#1437 = DIRECTION ( 'NONE',  ( 0.000000000000000000, 0.000000000000000000, 1.000000000000000000 ) ) ;
#1438 = ORIENTED_EDGE ( 'NONE', *, *, #20290, .F. ) ;
#1439 = EDGE_CURVE ( 'NONE', #13028, #8942, #18411, .T. ) ;
#1440 = CARTESIAN_POINT ( 'NONE',  ( 12.62672070884157804, -20.24999999999983658, 3.550922209436377042 ) ) ;
#1441 = VERTEX_POINT ( 'NONE', #9034 ) ;
#1442 = CARTESIAN_POINT ( 'NONE',  ( 1.707060460004204527, -9.864918773552613374, 2.372644200313257290 ) ) ;
#1443 = VERTEX_POINT ( 'NONE', #874 ) ;
#1444 = CARTESIAN_POINT ( 'NONE',  ( 9.722191417683177406, -20.27099543870833998, 4.275561207030583510 ) ) ;
#1445 = VECTOR ( 'NONE', #15787, 1000.000000000000000 ) ;
#1446 = DIRECTION ( 'NONE',  ( -0.000000000000000000, -0.000000000000000000, -1.000000000000000000 ) ) ;
#1447 = CARTESIAN_POINT ( 'NONE',  ( -1.896776615114361908, -10.21987218505477024, 2.463803327293850209 ) ) ;
#1448 = DIRECTION ( 'NONE',  ( 0.000000000000000000, 1.000000000000000000, 0.000000000000000000 ) ) ;
#1449 = CARTESIAN_POINT ( 'NONE',  ( -7.869520639128047002, 0.000000000000000000, 0.000000000000000000 ) ) ;
#1450 = ADVANCED_FACE ( 'NONE', ( #13828 ), #9233, .T. ) ;
#1451 = DIRECTION ( 'NONE',  ( 0.000000000000000000, 1.000000000000000000, 0.000000000000000000 ) ) ;
#1452 = CARTESIAN_POINT ( 'NONE',  ( 5.315941417683176518, -20.26807450282663225, 5.303608408759377113 ) ) ;
#1453 = CARTESIAN_POINT ( 'NONE',  ( -7.847191417683176518, -21.22443879296941915, 1.770995438708345748 ) ) ;
#1454 = ORIENTED_EDGE ( 'NONE', *, *, #17925, .F. ) ;
#1455 = CARTESIAN_POINT ( 'NONE',  ( 8.871558582316794173, -20.24999999999999289, 3.449312527122348371 ) ) ;
#1456 = CARTESIAN_POINT ( 'NONE',  ( -25.29469207716615031, 4.999999999999999112, 1.000000000000000000 ) ) ;
#1457 = CARTESIAN_POINT ( 'NONE',  ( -12.62500000000002132, -20.99999999999450395, 3.833333333368183382 ) ) ;
#1458 = VERTEX_POINT ( 'NONE', #1288 ) ;
#1459 = CARTESIAN_POINT ( 'NONE',  ( 6.340308582316793284, -22.67418626127525982, 5.270995438708342640 ) ) ;
#1460 = FACE_OUTER_BOUND ( 'NONE', #585, .T. ) ;
#1461 = VERTEX_POINT ( 'NONE', #20548 ) ;
#1462 = CARTESIAN_POINT ( 'NONE',  ( 10.18924542913430820, 11.64110105645932691, 0.000000000000000000 ) ) ;
#1463 = ORIENTED_EDGE ( 'NONE', *, *, #2388, .F. ) ;
#1464 = ADVANCED_FACE ( 'NONE', ( #12881 ), #14233, .T. ) ;
#1465 = LINE ( 'NONE', #20414, #442 ) ;
#1466 = ORIENTED_EDGE ( 'NONE', *, *, #3446, .T. ) ;
#1467 = CARTESIAN_POINT ( 'NONE',  ( -6.246558582316794173, -21.94931252712234482, 5.250000000000000888 ) ) ;
#1468 = CARTESIAN_POINT ( 'NONE',  ( -0.000000000000000000, 11.64110105645932691, 0.000000000000000000 ) ) ;
#1469 = FACE_OUTER_BOUND ( 'NONE', #6490, .T. ) ;
#1470 = CARTESIAN_POINT ( 'NONE',  ( 1.407845757905374695, -9.864917468222230923, 1.622643865078341907 ) ) ;
#1471 = ADVANCED_FACE ( 'NONE', ( #17386 ), #19074, .F. ) ;
#1472 = EDGE_CURVE ( 'NONE', #13772, #2830, #9444, .T. ) ;
#1473 = CARTESIAN_POINT ( 'NONE',  ( -15.00000000000000000, -6.000000000000000000, 2.000000000000000000 ) ) ;
#1474 = CARTESIAN_POINT ( 'NONE',  ( -13.74418849449709512, -0.8559810278826442964, 5.138499963383082125 ) ) ;
#1476 = CARTESIAN_POINT ( 'NONE',  ( 4.717959273841178636, -21.72818306014730183, 5.243595146365860771 ) ) ;
#1475 = AXIS2_PLACEMENT_3D ( 'NONE', #10527, #20476, #6132 ) ;
#1477 = CARTESIAN_POINT ( 'NONE',  ( -13.90434039801927568, 5.731690099970989216, 5.115558489342345361 ) ) ;
#1478 = CARTESIAN_POINT ( 'NONE',  ( 7.746558582316794173, -21.94931252712234482, 5.250000000000000888 ) ) ;
#1479 = CARTESIAN_POINT ( 'NONE',  ( 5.503441417683177406, -22.05068747287766229, 4.499999999999999112 ) ) ;
#1480 = CARTESIAN_POINT ( 'NONE',  ( -12.34719141768317741, -21.22443879296941915, 1.770995438708345748 ) ) ;
#1481 = B_SPLINE_CURVE_WITH_KNOTS ( 'NONE', 3,
 ( #3169, #1591, #1494, #12672, #18967, #4623, #11016, #14344, #7874, #4731, #28, #6415, #12780, #17808, #14766, #6919, #5352, #10263, #5459, #540, #8399, #19494, #9951, #16336, #19804, #2010, #11831, #5243, #10065, #11523 ),
 .UNSPECIFIED., .F., .F.,
 ( 4, 2, 2, 2, 2, 2, 2, 2, 2, 2, 2, 2, 2, 2, 4 ),
 ( 0.6080100341812841869, 0.6200887121040892236, 0.6309950902025724950, 0.6419014683010558775, 0.6637142244980225314, 0.7073397368919559502, 0.7509652492858893691, 0.7727780054828560230, 0.7836843835813394055, 0.7945907616798226769, 0.8074288390748337596, 0.8202669164698448423, 0.8459430712598670077, 0.8972953808399113385, 1.000000000000000000 ),
 .UNSPECIFIED. ) ;
#1482 = ORIENTED_EDGE ( 'NONE', *, *, #16635, .T. ) ;
#1483 = CARTESIAN_POINT ( 'NONE',  ( 13.38569699238614952, -18.95980188449660986, 4.749177046715717054 ) ) ;
#1484 = CARTESIAN_POINT ( 'NONE',  ( -1.126276606324276619, -9.114917468222230923, 1.622643865078341463 ) ) ;
#1485 = ORIENTED_EDGE ( 'NONE', *, *, #20231, .F. ) ;
#1486 = EDGE_CURVE ( 'NONE', #19789, #8535, #7778, .T. ) ;
#1487 = ORIENTED_EDGE ( 'NONE', *, *, #4376, .F. ) ;
#1488 = LINE ( 'NONE', #1796, #11778 ) ;
#1489 = CARTESIAN_POINT ( 'NONE',  ( -11.99999999999999467, -17.50000000000000000, 1.000000000000000000 ) ) ;
#1490 = CARTESIAN_POINT ( 'NONE',  ( -4.066879903460562495, -13.96783368734915776, 3.061584679647603391 ) ) ;
#1491 = DIRECTION ( 'NONE',  ( -0.000000000000000000, 0.000000000000000000, -1.000000000000000000 ) ) ;
#1492 = EDGE_CURVE ( 'NONE', #8225, #19576, #11119, .T. ) ;
#1493 = EDGE_CURVE ( 'NONE', #378, #6312, #19762, .T. ) ;
#1494 = CARTESIAN_POINT ( 'NONE',  ( 2.777355782919915139, -10.06396397089670458, 1.866377966073868411 ) ) ;
#1495 = CARTESIAN_POINT ( 'NONE',  ( -20.49999999999998224, -21.99999999999999645, 11.00000000000000178 ) ) ;
#1496 = CARTESIAN_POINT ( 'NONE',  ( 5.999999999999999112, -7.500000000000047073, 2.000000000000000000 ) ) ;
#1497 = CARTESIAN_POINT ( 'NONE',  ( 12.62500016093973620, -20.24999187254239175, 4.532396751752561848 ) ) ;
#1498 = CARTESIAN_POINT ( 'NONE',  ( -11.40969141768317918, -21.01515356694492098, 6.020995438708349745 ) ) ;
#1499 = CARTESIAN_POINT ( 'NONE',  ( -1.707060460004204527, -9.864918773552613374, 2.372644200313257290 ) ) ;
#1500 = ORIENTED_EDGE ( 'NONE', *, *, #3525, .F. ) ;
#1501 = CARTESIAN_POINT ( 'NONE',  ( -13.82092246150448211, 3.019084305971233562, 5.221833296715730377 ) ) ;
#1502 = CARTESIAN_POINT ( 'NONE',  ( 2.687849085826861995, 11.64110105645932691, 10.00000000000000000 ) ) ;
#1503 = CARTESIAN_POINT ( 'NONE',  ( 4.847191417683177406, -20.91377862118959285, 1.020995438708345082 ) ) ;
#1504 = CARTESIAN_POINT ( 'NONE',  ( -10.93405858231679595, -22.67126532539354855, 4.242948236979545484 ) ) ;
#1505 = ORIENTED_EDGE ( 'NONE', *, *, #18166, .T. ) ;
#1506 = CARTESIAN_POINT ( 'NONE',  ( 13.87470602645761986, 4.985154336109792972, 4.583333333333296622 ) ) ;
#1507 = CARTESIAN_POINT ( 'NONE',  ( 12.64131715375063258, -19.42598373559290792, 5.491151580003103660 ) ) ;
#1508 = CARTESIAN_POINT ( 'NONE',  ( 11.00000000000000000, -23.83493649053891517, 4.999999999999999112 ) ) ;
#1509 = EDGE_LOOP ( 'NONE', ( #2058, #14157, #12109, #10635 ) ) ;
#1510 = EDGE_CURVE ( 'NONE', #10510, #9451, #4528, .T. ) ;
#1511 = EDGE_LOOP ( 'NONE', ( #9435, #10300, #10130, #6368 ) ) ;
#1512 = CYLINDRICAL_SURFACE ( 'NONE', #10435, 1.499999999999996891 ) ;
#1513 = AXIS2_PLACEMENT_3D ( 'NONE', #3783, #7028, #19050 ) ;
#1514 = DIRECTION ( 'NONE',  ( 1.000000000000000000, 0.000000000000000000, 0.000000000000000000 ) ) ;
#1515 = ORIENTED_EDGE ( 'NONE', *, *, #6636, .F. ) ;
#1516 = FACE_BOUND ( 'NONE', #16320, .T. ) ;
#1517 = DIRECTION ( 'NONE',  ( -0.000000000000000000, -0.000000000000000000, -1.000000000000000000 ) ) ;
#1518 = DIRECTION ( 'NONE',  ( 0.000000000000000000, 1.000000000000000000, -0.000000000000000000 ) ) ;
#1519 = CARTESIAN_POINT ( 'NONE',  ( 0.2815691515810352374, -8.364917468222230923, 1.622643865078524428 ) ) ;
#1520 = LINE ( 'NONE', #19106, #4362 ) ;
#1521 = DIRECTION ( 'NONE',  ( 0.000000000000000000, -0.000000000000000000, 1.000000000000000000 ) ) ;
#1522 = CARTESIAN_POINT ( 'NONE',  ( 2.693754455098655409, -10.04853567022903782, 2.237415670251142519 ) ) ;
#1523 = DIRECTION ( 'NONE',  ( -1.000000000000000000, -1.192622389734054877E-16, 0.000000000000000000 ) ) ;
#1524 = CARTESIAN_POINT ( 'NONE',  ( -13.09030858231679417, -21.32581373872472597, 1.729004561291657582 ) ) ;
#1525 = CARTESIAN_POINT ( 'NONE',  ( -2.367358971471363649, -9.400572650371021410, 2.446005822389718087 ) ) ;
#1526 = MECHANICAL_DESIGN_GEOMETRIC_PRESENTATION_REPRESENTATION (  '', ( #14541 ), #509 ) ;
#1527 = CARTESIAN_POINT ( 'NONE',  ( 8.972191417683177406, -22.97900456129165292, 3.035098964749240125 ) ) ;
#1528 = CARTESIAN_POINT ( 'NONE',  ( -13.12529397354238192, 5.014845663890295846, 4.333333333333382775 ) ) ;
#1529 = CARTESIAN_POINT ( 'NONE',  ( -12.71530858231679240, -23.77099543870833998, 2.825813738724734847 ) ) ;
#1530 = CARTESIAN_POINT ( 'NONE',  ( -5.503441417683177406, -22.05068747287766229, 6.000000000000001776 ) ) ;
#1531 = ORIENTED_EDGE ( 'NONE', *, *, #8139, .T. ) ;
#1532 = CARTESIAN_POINT ( 'NONE',  ( 12.89855869007488209, -5.685286151195387383, 5.049178440009032265 ) ) ;
#1533 = FACE_OUTER_BOUND ( 'NONE', #19932, .T. ) ;
#1534 = ORIENTED_EDGE ( 'NONE', *, *, #3010, .T. ) ;
#1535 = CARTESIAN_POINT ( 'NONE',  ( 15.06494360078803041, 10.00000000000000000, 1.000000000000000000 ) ) ;
#1536 = ORIENTED_EDGE ( 'NONE', *, *, #15092, .T. ) ;
#1537 = DIRECTION ( 'NONE',  ( -1.000000000000000000, 0.000000000000000000, 0.000000000000000000 ) ) ;
#1538 = EDGE_CURVE ( 'NONE', #2967, #1461, #17489, .T. ) ;
#1539 = VECTOR ( 'NONE', #5300, 1000.000000000000000 ) ;
#1540 = ORIENTED_EDGE ( 'NONE', *, *, #16503, .F. ) ;
#1541 = DIRECTION ( 'NONE',  ( 1.000000000000000000, 0.000000000000000000, 0.000000000000000000 ) ) ;
#1542 = CARTESIAN_POINT ( 'NONE',  ( -28.94203811574919882, 16.00000000000000000, 1.000000000000000000 ) ) ;
#1543 = CARTESIAN_POINT ( 'NONE',  ( 0.000000000000000000, -9.864917468222230923, 2.372643865078341019 ) ) ;
#1544 = LINE ( 'NONE', #4680, #1021 ) ;
#1545 = CARTESIAN_POINT ( 'NONE',  ( -10.09030858231679417, -21.32581373872472952, 1.729004561291657138 ) ) ;
#1546 = CARTESIAN_POINT ( 'NONE',  ( 7.565941417683177406, -23.73192549717336064, 1.696391591240623331 ) ) ;
#1547 = CARTESIAN_POINT ( 'NONE',  ( -22.06633994409548194, 11.64110105645932691, 0.000000000000000000 ) ) ;
#1548 = CARTESIAN_POINT ( 'NONE',  ( -11.31594141768317741, -20.79840458871654363, 4.773278322869464851 ) ) ;
#1549 = ORIENTED_EDGE ( 'NONE', *, *, #1825, .F. ) ;
#1550 = CARTESIAN_POINT ( 'NONE',  ( 5.402808582316794173, -22.77556120703056308, 1.770995438708339975 ) ) ;
#1551 = LINE ( 'NONE', #19243, #17083 ) ;
#1552 = CARTESIAN_POINT ( 'NONE',  ( -13.04271272860988340, 0.09449279482665236263, 6.673537912489449830 ) ) ;
#1553 = ORIENTED_EDGE ( 'NONE', *, *, #6829, .T. ) ;
#1554 = AXIS2_PLACEMENT_3D ( 'NONE', #19099, #8305, #11236 ) ;
#1555 = CARTESIAN_POINT ( 'NONE',  ( 8.496558582316794173, -22.05068747287764452, 1.749999999999998446 ) ) ;
#1556 = CARTESIAN_POINT ( 'NONE',  ( 13.12500000000000000, 5.004982103124741677, 3.999999999999983569 ) ) ;
#1557 = ORIENTED_EDGE ( 'NONE', *, *, #15424, .F. ) ;
#1558 = LINE ( 'NONE', #1666, #5256 ) ;
#1559 = ORIENTED_EDGE ( 'NONE', *, *, #20383, .T. ) ;
#1560 = EDGE_CURVE ( 'NONE', #16909, #8663, #1704, .T. ) ;
#1561 = B_SPLINE_CURVE_WITH_KNOTS ( 'NONE', 3,
 ( #16574, #2154, #15119, #689, #16679, #8536, #8748, #2251, #13441, #7179, #13640, #19945, #14907, #8850, #5602, #8638, #15009, #11974, #19845, #18264, #5497, #4033, #15218, #10419, #13232, #16378, #10310, #8443, #19630, #9357, #9254, #18475, #15525, #4453, #14058, #5813, #4549, #2877, #15624, #16991, #5712, #6125, #16889, #12391, #7488, #1112, #13850, #20049, #2669, #12083, #4136, #10728, #15734, #20153, #998, #10518, #7388, #1211, #10837, #17201, #7690, #1311, #9056, #10932, #20466, #2559, #8945, #1415, #7797, #15318, #9157, #12494, #13751, #5911, #7586, #12183, #18573, #4236, #10617, #15427, #2780, #20252, #18888, #12282 ),
 .UNSPECIFIED., .F., .F.,
 ( 4, 2, 2, 2, 2, 2, 2, 2, 2, 2, 2, 2, 2, 2, 2, 2, 2, 2, 2, 2, 2, 2, 2, 2, 2, 2, 2, 2, 2, 2, 2, 2, 2, 2, 2, 2, 2, 2, 2, 2, 2, 4 ),
 ( 0.03313147696908362583, 0.03481082764294501225, 0.05122453910963482154, 0.05943139484297972619, 0.06353482270965217504, 0.06763825057632462390, 0.07081696859385247511, 0.07399568661138032633, 0.08035312264643602875, 0.09306799471654744749, 0.1057828667866588385, 0.1121403028217145548, 0.1153190208392423921, 0.1184977388567702433, 0.1214804596100246686, 0.1244631803632790662, 0.1304286218697878474, 0.1423595048828054654, 0.1662212709088405904, 0.2139448029609110069, 0.3093918670650517844, 0.5002859952733332838, 0.6911801234816148387, 0.7866271875857555607, 0.8343507196378260327, 0.8582124856638612131, 0.8701433686768788034, 0.8761088101833875985, 0.8790915309366421626, 0.8820742516898965047, 0.8853411830926055659, 0.8886081144953145161, 0.8951419773007326386, 0.9082097029115688835, 0.9212774285224051285, 0.9278112913278232510, 0.9310782227305320902, 0.9343451541332412624, 0.9384485819999136558, 0.9425520098665861601, 0.9507588655999309468, 0.9671725770666207422 ),
 .UNSPECIFIED. ) ;
#1562 = LINE ( 'NONE', #3235, #13129 ) ;
#1563 = ORIENTED_EDGE ( 'NONE', *, *, #16412, .F. ) ;
#1564 = CARTESIAN_POINT ( 'NONE',  ( -13.09030858231679417, -21.01515356694490322, 0.9790045612916562501 ) ) ;
#1565 = CARTESIAN_POINT ( 'NONE',  ( 4.000000000000000000, 0.000000000000000000, 0.000000000000000000 ) ) ;
#1566 = ADVANCED_FACE ( 'NONE', ( #17275 ), #12987, .F. ) ;
#1567 = FACE_OUTER_BOUND ( 'NONE', #5065, .T. ) ;
#1568 = CARTESIAN_POINT ( 'NONE',  ( 2.110348196723525138, -10.58007678474401914, 1.806311064303893099 ) ) ;
#1570 = EDGE_CURVE ( 'NONE', #1664, #16077, #9543, .T. ) ;
#1569 = VECTOR ( 'NONE', #6938, 1000.000000000000000 ) ;
#1571 = PLANE ( 'NONE',  #11672 ) ;
#1572 = CARTESIAN_POINT ( 'NONE',  ( -13.84500676459759383, 4.235341612176667603, 5.016097456370799179 ) ) ;
#1573 = CARTESIAN_POINT ( 'NONE',  ( 7.934058582316792396, -23.20159541128345992, 4.773278322869455970 ) ) ;
#1574 = CARTESIAN_POINT ( 'NONE',  ( -12.62499999999998224, -20.99999999999991829, 4.333333333333343695 ) ) ;
#1575 = CARTESIAN_POINT ( 'NONE',  ( -14.49999999999998579, -25.49999999999999645, 4.000000000000000000 ) ) ;
#1576 = CARTESIAN_POINT ( 'NONE',  ( -6.996558582316795949, -22.05068747287764452, 0.9999999999999978906 ) ) ;
#1577 = CARTESIAN_POINT ( 'NONE',  ( 9.152808582316794173, -21.22443879296942626, 5.229004561291659137 ) ) ;
#1578 = CARTESIAN_POINT ( 'NONE',  ( 6.815941417683177406, -21.32873467460645145, 4.242948236979555254 ) ) ;
#1579 = CARTESIAN_POINT ( 'NONE',  ( -6.434058582316794173, -23.20159541128345992, 4.773278322869455970 ) ) ;
#1580 = ORIENTED_EDGE ( 'NONE', *, *, #11475, .T. ) ;
#1581 = CARTESIAN_POINT ( 'NONE',  ( 13.84074239313819277, 4.019990853478630832, 5.241358430878110930 ) ) ;
#1582 = PLANE ( 'NONE',  #7681 ) ;
#1583 = VERTEX_POINT ( 'NONE', #134 ) ;
#1584 = EDGE_CURVE ( 'NONE', #16102, #14797, #3048, .T. ) ;
#1585 = ORIENTED_EDGE ( 'NONE', *, *, #1860, .F. ) ;
#1586 = LINE ( 'NONE', #4830, #2775 ) ;
#1587 = CARTESIAN_POINT ( 'NONE',  ( 0.6250000000000005551, 11.64110105645932691, 10.00000000000000000 ) ) ;
#1588 = CARTESIAN_POINT ( 'NONE',  ( -13.11017182064853159, 4.251176942750957366, 5.979809059808775196 ) ) ;
#1589 = CARTESIAN_POINT ( 'NONE',  ( -3.528325504133930313, -10.14411005961392398, 2.079576065490765124 ) ) ;
#1590 = DIRECTION ( 'NONE',  ( 0.000000000000000000, 0.000000000000000000, -1.000000000000000000 ) ) ;
#1591 = CARTESIAN_POINT ( 'NONE',  ( 2.781778019848414552, -10.09537774617444938, 1.874445651118397560 ) ) ;
#1592 = CARTESIAN_POINT ( 'NONE',  ( -12.64691428603184242, -19.14332855539073464, 5.509795676248469221 ) ) ;
#1593 = CARTESIAN_POINT ( 'NONE',  ( 10.46530858231679417, -20.22900456129164937, 4.174186261275266929 ) ) ;
#1594 = LINE ( 'NONE', #7781, #15066 ) ;
#1595 = CARTESIAN_POINT ( 'NONE',  ( 13.08107971211413378, 2.032025461757085427, 6.715204579155630960 ) ) ;
#1596 = EDGE_CURVE ( 'NONE', #2802, #18601, #3387, .T. ) ;
#1597 = CARTESIAN_POINT ( 'NONE',  ( -1.407845757905374695, -9.864917468222230923, 1.622643865078341907 ) ) ;
#1598 = ORIENTED_EDGE ( 'NONE', *, *, #17190, .F. ) ;
#1599 = CARTESIAN_POINT ( 'NONE',  ( -13.40022353639839103, -18.97621141187856608, 5.498856782956575984 ) ) ;
#1600 = LINE ( 'NONE', #38, #14047 ) ;
#1601 = VECTOR ( 'NONE', #13561, 1000.000000000000000 ) ;
#1602 = CARTESIAN_POINT ( 'NONE',  ( 7.940941417683175629, -20.19639159124061933, 1.768074502826635586 ) ) ;
#1603 = CARTESIAN_POINT ( 'NONE',  ( -4.565941417683176518, -22.67126532539353789, 2.757051763020445634 ) ) ;
#1604 = ORIENTED_EDGE ( 'NONE', *, *, #18607, .F. ) ;
#1605 = CARTESIAN_POINT ( 'NONE',  ( 13.87144757537903494, 4.070602556641903291, 6.741633940066556363 ) ) ;
#1606 = CARTESIAN_POINT ( 'NONE',  ( 12.64323021897839006, -19.32937394158751943, 5.504219675487169283 ) ) ;
#1607 = PLANE ( 'NONE',  #6334 ) ;
#1608 = VERTEX_POINT ( 'NONE', #14141 ) ;
#1609 = EDGE_CURVE ( 'NONE', #10227, #14087, #6299, .T. ) ;
#1610 = ORIENTED_EDGE ( 'NONE', *, *, #11754, .F. ) ;
#1611 = EDGE_CURVE ( 'NONE', #1939, #8942, #1481, .T. ) ;
#1612 = CARTESIAN_POINT ( 'NONE',  ( 10.38119784648305810, -14.00000000000000000, 1.000000000000000000 ) ) ;
#1613 = DIRECTION ( 'NONE',  ( 1.000000000000000000, 0.000000000000000000, 0.000000000000000000 ) ) ;
#1614 = VECTOR ( 'NONE', #5297, 1000.000000000000000 ) ;
#1615 = VECTOR ( 'NONE', #2064, 1000.000000000000000 ) ;
#1616 = DIRECTION ( 'NONE',  ( 0.000000000000000000, 0.000000000000000000, 1.000000000000000000 ) ) ;
#1617 = CARTESIAN_POINT ( 'NONE',  ( 2.513306525444908512, -9.622685169956881168, 2.503048754562789746 ) ) ;
#1618 = FACE_OUTER_BOUND ( 'NONE', #16736, .T. ) ;
#1619 = CARTESIAN_POINT ( 'NONE',  ( 0.000000000000000000, -9.864917468222230923, 1.622643865078341241 ) ) ;
#1620 = DIRECTION ( 'NONE',  ( -1.000000000000000000, -3.469446951953611033E-15, 0.000000000000000000 ) ) ;
#1621 = CARTESIAN_POINT ( 'NONE',  ( -5.999999999999999112, -7.500000000000047073, 9.999999999999998224 ) ) ;
#1622 = EDGE_CURVE ( 'NONE', #11456, #10835, #3473, .T. ) ;
#1623 = DIRECTION ( 'NONE',  ( 0.000000000000000000, -1.000000000000000000, 0.000000000000000000 ) ) ;
#1624 = DIRECTION ( 'NONE',  ( -0.000000000000000000, -0.000000000000000000, -1.000000000000000000 ) ) ;
#1625 = CARTESIAN_POINT ( 'NONE',  ( -11.59030858231679417, -21.32581373872472597, 1.729004561291657582 ) ) ;
#1626 = CARTESIAN_POINT ( 'NONE',  ( -2.875042468481914248, -11.91375063635796039, 3.091440134965714126 ) ) ;
#1627 = VECTOR ( 'NONE', #3594, 1000.000000000000000 ) ;
#1628 = CARTESIAN_POINT ( 'NONE',  ( 10.37155858231679595, -20.99999999999999645, 3.449312527122348371 ) ) ;
#1629 = CARTESIAN_POINT ( 'NONE',  ( -12.63238774201960268, -19.12691902800888499, 4.760115940007608515 ) ) ;
#1630 = CARTESIAN_POINT ( 'NONE',  ( -7.090308582316795061, -21.63647391050454871, 2.479004561291657804 ) ) ;
#1631 = CARTESIAN_POINT ( 'NONE',  ( -5.128441417683177406, -19.49999999999998934, 3.550687472877664952 ) ) ;
#1632 = VECTOR ( 'NONE', #7369, 1000.000000000000000 ) ;
#1633 = VERTEX_POINT ( 'NONE', #19689 ) ;
#1634 = CARTESIAN_POINT ( 'NONE',  ( 13.09560264575884503, 4.265433610975056133, 3.333333333333364568 ) ) ;
#1635 = LINE ( 'NONE', #2801, #17559 ) ;
#1636 = VERTEX_POINT ( 'NONE', #8285 ) ;
#1637 = VECTOR ( 'NONE', #15038, 1000.000000000000000 ) ;
#1638 = VERTEX_POINT ( 'NONE', #10165 ) ;
#1639 = CARTESIAN_POINT ( 'NONE',  ( 7.499999999999999112, -20.16506350946107418, 5.000000000000000000 ) ) ;
#1640 = CARTESIAN_POINT ( 'NONE',  ( 13.41175265982446696, -19.14399067886409256, 6.245281310864100988 ) ) ;
#1641 = ORIENTED_EDGE ( 'NONE', *, *, #13351, .F. ) ;
#1642 = CARTESIAN_POINT ( 'NONE',  ( 10.00000000000000533, -30.00000000000000355, 0.000000000000000000 ) ) ;
#1643 = B_SPLINE_CURVE_WITH_KNOTS ( 'NONE', 3,
 ( #10027, #11390, #5213, #8561, #19460, #1975, #11797, #5010, #14929, #11691, #8360, #18088, #410, #3850, #6996, #18186, #10230, #303, #16596, #609, #17974, #6793, #16406, #17776, #2081, #2274, #3443, #9822, #8466, #16207, #6690, #1873 ),
 .UNSPECIFIED., .F., .F.,
 ( 4, 2, 2, 2, 1, 2, 2, 2, 2, 2, 2, 2, 1, 2, 2, 2, 4 ),
 ( 0.5000677049534336671, 0.5625592418342705292, 0.5938050102746865733, 0.6094278944948945398, 0.6172393366049978569, 0.6211450576600495710, 0.6250507787151011740, 0.6875423155959299315, 0.7500338524767586890, 0.8125253893575872244, 0.8437711577980016031, 0.8593940420182086815, 0.8672054841283111104, 0.8711112051833602710, 0.8750169262384093205, 0.9375084631192046603, 1.000000000000000000 ),
 .UNSPECIFIED. ) ;
#1644 = AXIS2_PLACEMENT_3D ( 'NONE', #12595, #17830, #249 ) ;
#1645 = ORIENTED_EDGE ( 'NONE', *, *, #19492, .T. ) ;
#1646 = CARTESIAN_POINT ( 'NONE',  ( 10.94094141768317741, -20.72672167713052715, 2.298404588716546293 ) ) ;
#1647 = LINE ( 'NONE', #12619, #3950 ) ;
#1648 = AXIS2_PLACEMENT_3D ( 'NONE', #20610, #9197, #5956 ) ;
#1649 = CARTESIAN_POINT ( 'NONE',  ( -2.875042468481914248, -11.91375063635796039, 3.091440134965714126 ) ) ;
#1650 = DIRECTION ( 'NONE',  ( 0.000000000000000000, 0.1264857625231113059, 0.9919684228235025047 ) ) ;
#1651 = CARTESIAN_POINT ( 'NONE',  ( -11.21530858231679417, -23.77099543870833998, 2.825813738724734847 ) ) ;
#1652 = EDGE_CURVE ( 'NONE', #3666, #3062, #1902, .T. ) ;
#1653 = CARTESIAN_POINT ( 'NONE',  ( 6.159691417683175629, -22.98484643305507191, 0.9790045612916508100 ) ) ;
#1654 = CARTESIAN_POINT ( 'NONE',  ( 11.00000000000000000, -18.49999999999999645, 6.500000000000000888 ) ) ;
#1655 = CARTESIAN_POINT ( 'NONE',  ( -4.190941417683176518, -23.27327832286946219, 4.701595411283453707 ) ) ;
#1656 = ORIENTED_EDGE ( 'NONE', *, *, #17797, .T. ) ;
#1657 = CARTESIAN_POINT ( 'NONE',  ( 7.184058582316794173, -20.79840458871652942, 2.226721677130544030 ) ) ;
#1658 = FACE_OUTER_BOUND ( 'NONE', #18286, .T. ) ;
#1659 = CARTESIAN_POINT ( 'NONE',  ( -13.07148796623841847, 1.547642295024179493, 6.704787912489258872 ) ) ;
#1660 = ORIENTED_EDGE ( 'NONE', *, *, #8284, .T. ) ;
#1661 = CARTESIAN_POINT ( 'NONE',  ( 6.621558582316794173, -23.74999999999999645, 3.550687472877651629 ) ) ;
#1662 = LINE ( 'NONE', #17771, #14658 ) ;
#1663 = VECTOR ( 'NONE', #13515, 1000.000000000000000 ) ;
#1664 = VERTEX_POINT ( 'NONE', #443 ) ;
#1665 = PRODUCT ( 'spring', 'spring', '', ( #14521 ) ) ;
#1666 = CARTESIAN_POINT ( 'NONE',  ( -13.67791111847408025, 9.000000000000001776, 1.000000000000000000 ) ) ;
#1667 = APPLICATION_PROTOCOL_DEFINITION ( 'draft international standard', 'automotive_design', 1998, #7340 ) ;
#1668 = ORIENTED_EDGE ( 'NONE', *, *, #11266, .F. ) ;
#1669 = CARTESIAN_POINT ( 'NONE',  ( 11.00000000000000000, -20.16506350946107418, 5.000000000000000000 ) ) ;
#1670 = ORIENTED_EDGE ( 'NONE', *, *, #1949, .F. ) ;
#1671 = CARTESIAN_POINT ( 'NONE',  ( -12.62155858231679417, -24.50000000000000000, 3.550687472877651629 ) ) ;
#1672 = CARTESIAN_POINT ( 'NONE',  ( -15.00000000000000000, 0.000000000000000000, 1.000000000000000000 ) ) ;
#1673 = CARTESIAN_POINT ( 'NONE',  ( 24.50000000000000000, 3.000000000000000888, 0.000000000000000000 ) ) ;
#1674 = CARTESIAN_POINT ( 'NONE',  ( 2.327620134574780231, -13.27885108724501251, 3.249410218619480872 ) ) ;
#1675 = COLOUR_RGB ( '', 0.72549020, 0.75294118, 0.79215686) ;
#1676 = LINE ( 'NONE', #6085, #15019 ) ;
#1677 = CARTESIAN_POINT ( 'NONE',  ( -13.37499999998404121, -20.24999999996810729, 2.793053905886972998 ) ) ;
#1678 = CARTESIAN_POINT ( 'NONE',  ( 8.402808582316794173, -22.77556120703056308, 1.770995438708339975 ) ) ;
#1679 = CARTESIAN_POINT ( 'NONE',  ( -12.69740987707854707, -17.34330120752609616, 6.298537912489285517 ) ) ;
#1680 = STYLED_ITEM ( 'NONE', ( #6457 ), #11472 ) ;
#1681 = AXIS2_PLACEMENT_3D ( 'NONE', #12774, #4831, #3568 ) ;
#1682 = EDGE_CURVE ( 'NONE', #18231, #20454, #4041, .T. ) ;
#1683 = CARTESIAN_POINT ( 'NONE',  ( 4.068047865639286442, -21.69070144236915354, 4.840187030888444042 ) ) ;
#1684 = CARTESIAN_POINT ( 'NONE',  ( -10.37155858231679595, -19.49999999999998934, 3.449312527122348371 ) ) ;
#1685 = CARTESIAN_POINT ( 'NONE',  ( 6.715308582316794173, -23.77099543870833998, 2.825813738724734847 ) ) ;
#1686 = CARTESIAN_POINT ( 'NONE',  ( 5.409691417683178294, -21.63647391050456648, 4.520995438708348857 ) ) ;
#1687 = CARTESIAN_POINT ( 'NONE',  ( -6.815941417683176518, -20.79840458871654363, 4.773278322869464851 ) ) ;
#1688 = VERTEX_POINT ( 'NONE', #3572 ) ;
#1689 = VERTEX_POINT ( 'NONE', #15071 ) ;
#1690 = EDGE_CURVE ( 'NONE', #14252, #14385, #643, .T. ) ;
#1691 = CARTESIAN_POINT ( 'NONE',  ( 13.37499999999998224, -20.24999999999991829, 4.333333333333343695 ) ) ;
#1692 = ADVANCED_FACE ( 'NONE', ( #18220 ), #6822, .T. ) ;
#1693 = CARTESIAN_POINT ( 'NONE',  ( -22.85856191738413656, 4.999999999999999112, 1.000000000000000000 ) ) ;
#1694 = CARTESIAN_POINT ( 'NONE',  ( 24.62918902992234038, 10.00000000000000000, 1.000000000000000000 ) ) ;
#1695 = ORIENTED_EDGE ( 'NONE', *, *, #9410, .F. ) ;
#1696 = PRODUCT_DEFINITION_FORMATION_WITH_SPECIFIED_SOURCE ( 'ANY', '', #6339, .NOT_KNOWN. ) ;
#1697 = ORIENTED_EDGE ( 'NONE', *, *, #12211, .F. ) ;
#1698 = DIRECTION ( 'NONE',  ( -1.000000000000000000, 0.000000000000000000, 0.000000000000000000 ) ) ;
#1699 = DIRECTION ( 'NONE',  ( 1.000000000000000000, 0.000000000000000000, -0.000000000000000000 ) ) ;
#1700 = VECTOR ( 'NONE', #16899, 1000.000000000000000 ) ;
#1701 = FACE_OUTER_BOUND ( 'NONE', #10294, .T. ) ;
#1702 = CARTESIAN_POINT ( 'NONE',  ( -1.743623630681728542, -9.116095536440919744, 2.372946416531167557 ) ) ;
#1703 = CARTESIAN_POINT ( 'NONE',  ( 16.37779268661489596, 16.00000000000000000, 1.000000000000000000 ) ) ;
#1704 = LINE ( 'NONE', #8188, #12056 ) ;
#1705 = CARTESIAN_POINT ( 'NONE',  ( -12.62515553039088090, -20.24214571525854467, 4.629702272822510345 ) ) ;
#1706 = LINE ( 'NONE', #16030, #3419 ) ;
#1707 = DIRECTION ( 'NONE',  ( 1.000000000000000000, 0.000000000000000000, 0.000000000000000000 ) ) ;
#1708 = CARTESIAN_POINT ( 'NONE',  ( 12.62499999999998579, -20.24999999999999289, 3.146526952850934755 ) ) ;
#1709 = EDGE_CURVE ( 'NONE', #17379, #20661, #13091, .T. ) ;
#1710 = CARTESIAN_POINT ( 'NONE',  ( -1.772926875221950249, -9.883376166076789815, 2.377384427436886494 ) ) ;
#1711 = ORIENTED_EDGE ( 'NONE', *, *, #2479, .F. ) ;
#1712 = CARTESIAN_POINT ( 'NONE',  ( -13.85788212999909419, 4.135547564954428879, 5.982801014393342776 ) ) ;
#1713 = CARTESIAN_POINT ( 'NONE',  ( 13.49999999999998401, -19.52007894294123957, 12.00000000000000000 ) ) ;
#1714 = VECTOR ( 'NONE', #10709, 1000.000000000000000 ) ;
#1715 = CARTESIAN_POINT ( 'NONE',  ( 5.315941417683176518, -20.26807450282663225, 5.303608408759377113 ) ) ;
#1716 = CARTESIAN_POINT ( 'NONE',  ( -10.46530858231679595, -20.97900456129165647, 3.863526089495444626 ) ) ;
#1717 = ORIENTED_EDGE ( 'NONE', *, *, #4886, .T. ) ;
#1718 = AXIS2_PLACEMENT_3D ( 'NONE', #11317, #19284, #6518 ) ;
#1719 = CARTESIAN_POINT ( 'NONE',  ( 13.86316420010827777, 3.652292105464413297, 6.735515685864076119 ) ) ;
#1720 = CARTESIAN_POINT ( 'NONE',  ( 12.79798428357658047, -11.51429367935891790, 5.673858176248284479 ) ) ;
#1721 = DIRECTION ( 'NONE',  ( -1.000000000000000000, 0.000000000000000000, 0.000000000000000000 ) ) ;
#1722 = EDGE_LOOP ( 'NONE', ( #20152, #4422, #12846, #17772 ) ) ;
#1723 = ORIENTED_EDGE ( 'NONE', *, *, #4575, .F. ) ;
#1724 = CARTESIAN_POINT ( 'NONE',  ( 7.499999999999999112, -23.83493649053891517, 4.999999999999999112 ) ) ;
#1725 = DIRECTION ( 'NONE',  ( 1.000000000000000000, 0.000000000000000000, 0.000000000000000000 ) ) ;
#1726 = CARTESIAN_POINT ( 'NONE',  ( -26.04469207716615031, 9.000000000000001776, 0.000000000000000000 ) ) ;
#1727 = AXIS2_PLACEMENT_3D ( 'NONE', #17344, #1355, #11272 ) ;
#1728 = LINE ( 'NONE', #3193, #10664 ) ;
#1729 = CARTESIAN_POINT ( 'NONE',  ( 2.011668220304084542, -11.03559989230542193, 2.673298498313999794 ) ) ;
#1730 = LINE ( 'NONE', #12597, #15873 ) ;
#1731 = CARTESIAN_POINT ( 'NONE',  ( 0.000000000000000000, 10.00000000000000000, 1.000000000000000000 ) ) ;
#1732 = EDGE_CURVE ( 'NONE', #3797, #7379, #13191, .T. ) ;
#1733 = DIRECTION ( 'NONE',  ( -0.000000000000000000, -0.000000000000000000, -1.000000000000000000 ) ) ;
#1734 = LINE ( 'NONE', #14377, #15987 ) ;
#1735 = CARTESIAN_POINT ( 'NONE',  ( -2.693754455098655409, -9.955255285363838524, 2.600628789231445470 ) ) ;
#1736 = EDGE_CURVE ( 'NONE', #11041, #2445, #5146, .T. ) ;
#1737 = CARTESIAN_POINT ( 'NONE',  ( -2.817596665886821672, -11.50588678273290988, 2.986692549455723267 ) ) ;
#1738 = CARTESIAN_POINT ( 'NONE',  ( 9.527808582316795949, -22.97900456129165647, 3.964901035250747885 ) ) ;
#1739 = CARTESIAN_POINT ( 'NONE',  ( -13.09173631808601002, 4.070184063342107805, 5.250510817581989009 ) ) ;
#1740 = CARTESIAN_POINT ( 'NONE',  ( -12.90280858231679773, -22.77556120703056308, 1.770995438708339975 ) ) ;
#1741 = CARTESIAN_POINT ( 'NONE',  ( -10.28469141768318096, -23.77099543870834353, 4.174186261275252718 ) ) ;
#1742 = VERTEX_POINT ( 'NONE', #13398 ) ;
#1743 = CARTESIAN_POINT ( 'NONE',  ( 13.84439157666246878, 4.204274621457510186, 5.123803251657143676 ) ) ;
#1744 = LINE ( 'NONE', #11252, #18740 ) ;
#1745 = ORIENTED_EDGE ( 'NONE', *, *, #19077, .T. ) ;
#1746 = ORIENTED_EDGE ( 'NONE', *, *, #2905, .F. ) ;
#1747 = VECTOR ( 'NONE', #1848, 1000.000000000000000 ) ;
#1748 = LINE ( 'NONE', #19628, #2042 ) ;
#1749 = ORIENTED_EDGE ( 'NONE', *, *, #17411, .T. ) ;
#1750 = CARTESIAN_POINT ( 'NONE',  ( 5.683390479346035029, 4.999999999999999112, 1.000000000000000000 ) ) ;
#1751 = ORIENTED_EDGE ( 'NONE', *, *, #17024, .F. ) ;
#1752 = VECTOR ( 'NONE', #18473, 1000.000000000000000 ) ;
#1753 = CARTESIAN_POINT ( 'NONE',  ( 8.690941417683177406, -23.27327832286946219, 4.701595411283453707 ) ) ;
#1754 = DIRECTION ( 'NONE',  ( 1.000000000000000000, 0.000000000000000000, 0.000000000000000000 ) ) ;
#1755 = CARTESIAN_POINT ( 'NONE',  ( -1.407845757905374695, -9.864917468222230923, 2.372643865078341019 ) ) ;
#1756 = DIRECTION ( 'NONE',  ( 1.000000000000000000, 0.000000000000000000, 0.000000000000000000 ) ) ;
#1757 = CARTESIAN_POINT ( 'NONE',  ( -12.62155858231679417, -23.74999999999999645, 3.550687472877651629 ) ) ;
#1758 = VECTOR ( 'NONE', #11337, 1000.000000000000000 ) ;
#1759 = CARTESIAN_POINT ( 'NONE',  ( 6.347191417683176518, -21.22443879296941915, 1.770995438708345748 ) ) ;
#1760 = FACE_OUTER_BOUND ( 'NONE', #11634, .T. ) ;
#1761 = CARTESIAN_POINT ( 'NONE',  ( -11.40969141768317918, -21.63647391050456648, 4.520995438708348857 ) ) ;
#1762 = ORIENTED_EDGE ( 'NONE', *, *, #7611, .F. ) ;
#1763 = CARTESIAN_POINT ( 'NONE',  ( 11.12155858231679595, -24.50000000000000000, 3.550687472877651629 ) ) ;
#1764 = CARTESIAN_POINT ( 'NONE',  ( 12.62524871736568954, -20.23743977303344010, 4.661898514667671023 ) ) ;
#1765 = CARTESIAN_POINT ( 'NONE',  ( -13.14782865898149034, 5.402847278557675104, 6.092770214907355708 ) ) ;
#1766 = ORIENTED_EDGE ( 'NONE', *, *, #20416, .T. ) ;
#1767 = LINE ( 'NONE', #8155, #14956 ) ;
#1768 = CARTESIAN_POINT ( 'NONE',  ( 9.555650798910054533, 0.000000000000000000, 0.000000000000000000 ) ) ;
#1769 = ORIENTED_EDGE ( 'NONE', *, *, #19488, .F. ) ;
#1770 = VERTEX_POINT ( 'NONE', #14962 ) ;
#1771 = CIRCLE ( 'NONE', #7777, 1.000000000000002665 ) ;
#1772 = EDGE_CURVE ( 'NONE', #4081, #14620, #2311, .T. ) ;
#1773 = LINE ( 'NONE', #17248, #15470 ) ;
#1774 = ORIENTED_EDGE ( 'NONE', *, *, #5845, .F. ) ;
#1775 = CARTESIAN_POINT ( 'NONE',  ( -5.402808582316794173, -22.77556120703056308, 1.770995438708339975 ) ) ;
#1776 = DIRECTION ( 'NONE',  ( -1.000000000000000000, 0.000000000000000000, 0.000000000000000000 ) ) ;
#1777 = DIRECTION ( 'NONE',  ( 0.000000000000000000, -0.9659258262890672020, 0.2588190451025245142 ) ) ;
#1778 = CARTESIAN_POINT ( 'NONE',  ( 2.124709647372160060, -10.68204274815009924, 1.832497960681391147 ) ) ;
#1779 = CARTESIAN_POINT ( 'NONE',  ( 12.62500000000001954, -20.24999999999450040, 3.833333333368183382 ) ) ;
#1780 = CARTESIAN_POINT ( 'NONE',  ( -23.35856191738413656, 4.999999999999999112, 0.000000000000000000 ) ) ;
#1781 = CARTESIAN_POINT ( 'NONE',  ( -13.84501474873290938, 4.235744811019327649, 4.974109985360144037 ) ) ;
#1782 = CARTESIAN_POINT ( 'NONE',  ( 9.434058582316795949, -23.73192549717337130, 5.303608408759367343 ) ) ;
#1783 = CARTESIAN_POINT ( 'NONE',  ( -13.15469878640066526, 5.749788713235649773, 5.232478742873432509 ) ) ;
#1784 = CIRCLE ( 'NONE', #2435, 10.00000000000000000 ) ;
#1785 = DIRECTION ( 'NONE',  ( 0.000000000000000000, 0.000000000000000000, 1.000000000000000000 ) ) ;
#1786 = CARTESIAN_POINT ( 'NONE',  ( 6.902808582316793284, -22.77556120703056308, 1.770995438708339975 ) ) ;
#1787 = CARTESIAN_POINT ( 'NONE',  ( 8.972191417683177406, -22.97900456129165292, 3.035098964749240125 ) ) ;
#1788 = CARTESIAN_POINT ( 'NONE',  ( -4.753441417683176518, -21.94931252712233061, 1.749999999999998446 ) ) ;
#1789 = ORIENTED_EDGE ( 'NONE', *, *, #16619, .T. ) ;
#1790 = ORIENTED_EDGE ( 'NONE', *, *, #11684, .T. ) ;
#1791 = CARTESIAN_POINT ( 'NONE',  ( 13.37499979530394967, -20.25001033714808329, 4.458488164327452097 ) ) ;
#1792 = CARTESIAN_POINT ( 'NONE',  ( 0.000000000000000000, 11.64110105645932691, 10.00000000000000000 ) ) ;
#1793 = CARTESIAN_POINT ( 'NONE',  ( 0.000000000000000000, 0.000000000000000000, 0.000000000000000000 ) ) ;
#1794 = ORIENTED_EDGE ( 'NONE', *, *, #2779, .F. ) ;
#1795 = ORIENTED_EDGE ( 'NONE', *, *, #10684, .T. ) ;
#1796 = CARTESIAN_POINT ( 'NONE',  ( -19.48630159782011262, 9.000000000000001776, 1.000000000000000000 ) ) ;
#1797 = CARTESIAN_POINT ( 'NONE',  ( 14.50000000000001243, -18.49999999999999645, 1.000000000000000000 ) ) ;
#1798 = EDGE_CURVE ( 'NONE', #15962, #4449, #8495, .T. ) ;
#1799 = PLANE ( 'NONE',  #15935 ) ;
#1800 = CARTESIAN_POINT ( 'NONE',  ( -0.5631383031621635116, -8.364917468222230923, 1.622643865078341907 ) ) ;
#1801 = DIRECTION ( 'NONE',  ( 1.000000000000000000, -0.000000000000000000, 0.000000000000000000 ) ) ;
#1802 = EDGE_CURVE ( 'NONE', #1213, #6097, #2210, .T. ) ;
#1803 = DIRECTION ( 'NONE',  ( -1.000000000000000000, -0.000000000000000000, -0.000000000000000000 ) ) ;
#1804 = CARTESIAN_POINT ( 'NONE',  ( -12.64751377014909828, -19.11305460747000495, 5.510446717915143289 ) ) ;
#1805 = DIRECTION ( 'NONE',  ( -0.000000000000000000, -0.000000000000000000, -1.000000000000000000 ) ) ;
#1806 = EDGE_CURVE ( 'NONE', #3359, #14333, #8700, .T. ) ;
#1807 = LINE ( 'NONE', #6108, #14741 ) ;
#1808 = CARTESIAN_POINT ( 'NONE',  ( 13.15498530132288479, 5.764257716805535559, 4.791666666666684726 ) ) ;
#1809 = CARTESIAN_POINT ( 'NONE',  ( -2.041623931606483033, -10.12028065167953272, 1.688226231982305370 ) ) ;
#1810 = ORIENTED_EDGE ( 'NONE', *, *, #17827, .F. ) ;
#1811 = CARTESIAN_POINT ( 'NONE',  ( -13.49014615398506045, -14.43511922376608680, 5.596513032956658584 ) ) ;
#1812 = FACE_OUTER_BOUND ( 'NONE', #16104, .T. ) ;
#1813 = CARTESIAN_POINT ( 'NONE',  ( 7.659691417683177406, -22.98484643305507191, 0.9790045612916508100 ) ) ;
#1814 = CARTESIAN_POINT ( 'NONE',  ( -5.684058582316795949, -21.32873467460644079, 2.757051763020455404 ) ) ;
#1815 = ORIENTED_EDGE ( 'NONE', *, *, #1074, .F. ) ;
#1816 = CARTESIAN_POINT ( 'NONE',  ( 13.90439735423812273, 5.734566389025032684, 2.999999999999999556 ) ) ;
#1817 = CARTESIAN_POINT ( 'NONE',  ( 13.10431844137356627, 3.955581289335645234, 6.006545679920360925 ) ) ;
#1818 = LINE ( 'NONE', #17918, #2993 ) ;
#1819 = ORIENTED_EDGE ( 'NONE', *, *, #6500, .T. ) ;
#1820 = ORIENTED_EDGE ( 'NONE', *, *, #15526, .F. ) ;
#1821 = DIRECTION ( 'NONE',  ( -1.000000000000000000, 0.000000000000000000, 0.000000000000000000 ) ) ;
#1822 = EDGE_CURVE ( 'NONE', #16179, #9059, #11423, .T. ) ;
#1823 = DIRECTION ( 'NONE',  ( -0.000000000000000000, 0.000000000000000000, 1.000000000000000000 ) ) ;
#1824 = ORIENTED_EDGE ( 'NONE', *, *, #16454, .T. ) ;
#1825 = EDGE_CURVE ( 'NONE', #8456, #2576, #5382, .T. ) ;
#1826 = CARTESIAN_POINT ( 'NONE',  ( 11.00000000000000000, -20.16506350946107418, 5.000000000000000000 ) ) ;
#1827 = CARTESIAN_POINT ( 'NONE',  ( 1.982945319006538032, -10.83166796549307520, 2.620924705558935308 ) ) ;
#1828 = CARTESIAN_POINT ( 'NONE',  ( 12.00000000000000178, -26.50000000000000355, 4.000000000000000000 ) ) ;
#1829 = ADVANCED_FACE ( 'NONE', ( #1268 ), #3988, .T. ) ;
#1830 = DIRECTION ( 'NONE',  ( 1.000000000000000000, 0.000000000000000000, 0.000000000000000000 ) ) ;
#1831 = LINE ( 'NONE', #161, #18030 ) ;
#1832 = CARTESIAN_POINT ( 'NONE',  ( 15.00000000000001421, -25.49999999999999645, 1.000000000000000000 ) ) ;
#1833 = CARTESIAN_POINT ( 'NONE',  ( -10.93405858231679417, -23.20159541128345992, 4.773278322869455970 ) ) ;
#1834 = CARTESIAN_POINT ( 'NONE',  ( -12.62672070884157804, -20.24999999999991473, 3.550922209436377042 ) ) ;
#1835 = PRODUCT ( 'BR-832', 'BR-832', '', ( #3335 ) ) ;
#1836 = ORIENTED_EDGE ( 'NONE', *, *, #5658, .T. ) ;
#1837 = CARTESIAN_POINT ( 'NONE',  ( -12.62599452815238443, -19.44977632830967806, 4.656396506304353977 ) ) ;
#1838 = CARTESIAN_POINT ( 'NONE',  ( -11.96530858231679595, -20.22900456129164937, 4.174186261275266929 ) ) ;
#1839 = CARTESIAN_POINT ( 'NONE',  ( -8.222191417683175629, -20.27099543870833998, 4.275561207030583510 ) ) ;
#1840 = ORIENTED_EDGE ( 'NONE', *, *, #9665, .F. ) ;
#1841 = CARTESIAN_POINT ( 'NONE',  ( 13.79214722387705905, 1.565934805775630601, 5.190583296715636230 ) ) ;
#1843 = DIRECTION ( 'NONE',  ( -1.000000000000000000, -1.192622389734054877E-16, 0.000000000000000000 ) ) ;
#1842 = VECTOR ( 'NONE', #7752, 1000.000000000000000 ) ;
#1844 = VERTEX_POINT ( 'NONE', #15484 ) ;
#1845 = ORIENTED_EDGE ( 'NONE', *, *, #9443, .T. ) ;
#1846 = DIRECTION ( 'NONE',  ( 0.000000000000000000, -0.9659258262890672020, 0.2588190451025246253 ) ) ;
#1847 = VERTEX_POINT ( 'NONE', #852 ) ;
#1848 = DIRECTION ( 'NONE',  ( -1.000000000000000000, -1.156482317317871725E-16, -0.000000000000000000 ) ) ;
#1849 = EDGE_CURVE ( 'NONE', #14060, #19940, #8808, .T. ) ;
#1850 = AXIS2_PLACEMENT_3D ( 'NONE', #20670, #3289, #19308 ) ;
#1851 = VERTEX_POINT ( 'NONE', #4297 ) ;
#1852 = CARTESIAN_POINT ( 'NONE',  ( 11.59719141768317563, -22.77556120703057729, 5.229004561291656472 ) ) ;
#1853 = CARTESIAN_POINT ( 'NONE',  ( -0.000000000000000000, 10.00000000000000000, 0.000000000000000000 ) ) ;
#1854 = CARTESIAN_POINT ( 'NONE',  ( -3.047379876266447685, -13.13734219723468755, 3.405682891496055742 ) ) ;
#1855 = CARTESIAN_POINT ( 'NONE',  ( 2.436080212393455735, -9.483920418190111334, 2.467411194204634839 ) ) ;
#1856 = CARTESIAN_POINT ( 'NONE',  ( -11.68405858231679417, -20.79840458871652942, 2.226721677130544030 ) ) ;
#1857 = FILL_AREA_STYLE_COLOUR ( '', #17300 ) ;
#1858 = CARTESIAN_POINT ( 'NONE',  ( 8.222191417683175629, -20.27099543870833998, 4.275561207030583510 ) ) ;
#1859 = PLANE ( 'NONE',  #6196 ) ;
#1860 = EDGE_CURVE ( 'NONE', #20119, #8195, #13809, .T. ) ;
#1861 = CARTESIAN_POINT ( 'NONE',  ( -10.28469141768317741, -23.02099543870834353, 3.863526089495429972 ) ) ;
#1862 = ORIENTED_EDGE ( 'NONE', *, *, #19649, .F. ) ;
#1863 = CARTESIAN_POINT ( 'NONE',  ( 8.871558582316795949, -19.49999999999998934, 3.449312527122348371 ) ) ;
#1864 = CARTESIAN_POINT ( 'NONE',  ( 12.62500000000001954, -20.24999999999450040, 3.833333333368183382 ) ) ;
#1865 = CARTESIAN_POINT ( 'NONE',  ( -13.15498530132288479, 5.764257716805535559, 4.166666666666765551 ) ) ;
#1866 = VERTEX_POINT ( 'NONE', #5666 ) ;
#1867 = LINE ( 'NONE', #16401, #20324 ) ;
#1868 = DIRECTION ( 'NONE',  ( 1.000000000000000000, 0.000000000000000000, 0.000000000000000000 ) ) ;
#1869 = EDGE_LOOP ( 'NONE', ( #11250, #11872, #14832, #4061 ) ) ;
#1870 = CARTESIAN_POINT ( 'NONE',  ( 0.000000000000000000, 0.000000000000000000, 0.000000000000000000 ) ) ;
#1871 = ORIENTED_EDGE ( 'NONE', *, *, #10640, .F. ) ;
#1872 = EDGE_CURVE ( 'NONE', #4053, #6506, #19903, .T. ) ;
#1873 = CARTESIAN_POINT ( 'NONE',  ( 12.62672070884157804, -20.24999999999983658, 3.550922209436377042 ) ) ;
#1874 = EDGE_CURVE ( 'NONE', #11254, #11965, #7546, .T. ) ;
#1875 = ORIENTED_EDGE ( 'NONE', *, *, #10161, .F. ) ;
#1876 = CARTESIAN_POINT ( 'NONE',  ( -11.68405858231679595, -20.26807450282662160, 1.696391591240633101 ) ) ;
#1877 = CARTESIAN_POINT ( 'NONE',  ( 13.09892531043291086, 3.683228176858501790, 6.000681092915118420 ) ) ;
#1878 = CYLINDRICAL_SURFACE ( 'NONE', #12140, 1.499999999999999556 ) ;
#1879 = AXIS2_PLACEMENT_3D ( 'NONE', #7536, #2829, #7437 ) ;
#1880 = SHAPE_REPRESENTATION ( 'BR-832', ( #8040, #18, #18060, #19065, #17728, #8709 ), #5692 ) ;
#1881 = CARTESIAN_POINT ( 'NONE',  ( 12.64571531779736979, -19.20387645123237164, 5.508493592915143289 ) ) ;
#1882 = DIRECTION ( 'NONE',  ( 0.000000000000000000, 0.000000000000000000, 1.000000000000000000 ) ) ;
#1883 = CARTESIAN_POINT ( 'NONE',  ( -13.40368151590352497, -18.05158344687463412, 4.768708296715732153 ) ) ;
#1884 = CARTESIAN_POINT ( 'NONE',  ( 7.746558582316795949, -21.94931252712234127, 6.000000000000001776 ) ) ;
#1885 = CARTESIAN_POINT ( 'NONE',  ( -13.15498501280115917, 5.764243146453090105, 5.045733045595949484 ) ) ;
#1886 = EDGE_CURVE ( 'NONE', #200, #2500, #20000, .T. ) ;
#1887 = CARTESIAN_POINT ( 'NONE',  ( -10.19094141768317741, -23.80360840875937001, 5.231925497173365081 ) ) ;
#1888 = PLANE ( 'NONE',  #11720 ) ;
#1889 = LINE ( 'NONE', #18105, #20451 ) ;
#1890 = CARTESIAN_POINT ( 'NONE',  ( 10.55905858231679595, -21.25705176302045274, 4.171265325393551215 ) ) ;
#1891 = CARTESIAN_POINT ( 'NONE',  ( -7.847191417683176518, -21.22443879296941915, 1.770995438708345748 ) ) ;
#1892 = ORIENTED_EDGE ( 'NONE', *, *, #6039, .T. ) ;
#1893 = ORIENTED_EDGE ( 'NONE', *, *, #3662, .F. ) ;
#1894 = CARTESIAN_POINT ( 'NONE',  ( 13.37499999998404121, -20.24999999996810729, 2.793053905886972998 ) ) ;
#1895 = DIRECTION ( 'NONE',  ( 0.000000000000000000, 1.000000000000000000, -0.000000000000000000 ) ) ;
#1896 = ORIENTED_EDGE ( 'NONE', *, *, #3165, .T. ) ;
#1897 = ORIENTED_EDGE ( 'NONE', *, *, #3339, .T. ) ;
#1898 = CARTESIAN_POINT ( 'NONE',  ( 24.62918902992234038, 11.64110105645932691, 10.00000000000000000 ) ) ;
#1899 = CARTESIAN_POINT ( 'NONE',  ( -13.49999999999998401, -21.99999999999999645, 14.18378559369222280 ) ) ;
#1900 = LINE ( 'NONE', #11214, #20633 ) ;
#1901 = DIRECTION ( 'NONE',  ( 0.000000000000000000, 0.000000000000000000, 1.000000000000000000 ) ) ;
#1902 = LINE ( 'NONE', #16236, #16080 ) ;
#1903 = CARTESIAN_POINT ( 'NONE',  ( -12.79798428357658047, -11.51429367935891790, 5.673858176248284479 ) ) ;
#1904 = CARTESIAN_POINT ( 'NONE',  ( 9.059058582316794173, -20.72672167713054137, 4.701595411283463477 ) ) ;
#1905 = CARTESIAN_POINT ( 'NONE',  ( 0.000000000000000000, 10.00000000000000000, 1.000000000000000000 ) ) ;
#1906 = CARTESIAN_POINT ( 'NONE',  ( 12.62745083560477966, -20.12623280195927933, 5.001038150054709419 ) ) ;
#1907 = EDGE_CURVE ( 'NONE', #17851, #19480, #5772, .T. ) ;
#1908 = DIRECTION ( 'NONE',  ( 1.000000000000000000, -0.000000000000000000, 0.000000000000000000 ) ) ;
#1909 = ORIENTED_EDGE ( 'NONE', *, *, #15811, .T. ) ;
#1910 = AXIS2_PLACEMENT_3D ( 'NONE', #9537, #3065, #12980 ) ;
#1911 = CARTESIAN_POINT ( 'NONE',  ( -13.86693669322925260, 4.592803008081209448, 5.801483467520450077 ) ) ;
#1912 = DIRECTION ( 'NONE',  ( 1.734723475976809560E-16, -1.000000000000000000, 0.000000000000000000 ) ) ;
#1913 = EDGE_CURVE ( 'NONE', #740, #4847, #10793, .T. ) ;
#1914 = CARTESIAN_POINT ( 'NONE',  ( 9.253441417683177406, -21.94931252712233061, 1.749999999999998446 ) ) ;
#1915 = CARTESIAN_POINT ( 'NONE',  ( -8.965308582316795949, -20.97900456129165647, 3.863526089495444626 ) ) ;
#1916 = ORIENTED_EDGE ( 'NONE', *, *, #8465, .F. ) ;
#1917 = CARTESIAN_POINT ( 'NONE',  ( 13.90439735423812273, 5.734566389025032684, 4.916666666666649199 ) ) ;
#1918 = CARTESIAN_POINT ( 'NONE',  ( 13.12503131243110843, 5.001581277770153378, 5.166347330538456184 ) ) ;
#1919 = CARTESIAN_POINT ( 'NONE',  ( -13.19540963423371949, -19.91531415481216882, 3.473342506385693085 ) ) ;
#1920 = EDGE_LOOP ( 'NONE', ( #602, #17525, #19374, #11232, #9716 ) ) ;
#1921 = ORIENTED_EDGE ( 'NONE', *, *, #12222, .T. ) ;
#1922 = DIRECTION ( 'NONE',  ( -1.000000000000000000, 0.000000000000000000, 0.000000000000000000 ) ) ;
#1923 = PLANE ( 'NONE',  #2904 ) ;
#1924 = CARTESIAN_POINT ( 'NONE',  ( -15.49999999999999822, -20.99999999999999645, 4.000000000000000000 ) ) ;
#1925 = CARTESIAN_POINT ( 'NONE',  ( 1.811130159782011528, 9.000000000000001776, 1.000000000000000000 ) ) ;
#1926 = CARTESIAN_POINT ( 'NONE',  ( 1.862510824048270619, -9.990417728039201251, 2.404874838918925395 ) ) ;
#1927 = CARTESIAN_POINT ( 'NONE',  ( -5.381197846483055436, -6.000000000000000000, 1.000000000000000000 ) ) ;
#1928 = CARTESIAN_POINT ( 'NONE',  ( 0.3749999999999968914, 9.000000000000000000, 1.000000000000000000 ) ) ;
#1929 = AXIS2_PLACEMENT_3D ( 'NONE', #10642, #15450, #16810 ) ;
#1930 = DIRECTION ( 'NONE',  ( 1.000000000000000000, 0.000000000000000000, 0.000000000000000000 ) ) ;
#1931 = DIRECTION ( 'NONE',  ( -0.000000000000000000, -0.000000000000000000, -1.000000000000000000 ) ) ;
#1932 = CARTESIAN_POINT ( 'NONE',  ( -13.37155858231679417, -20.24999999999999289, 3.449312527122348371 ) ) ;
#1933 = CARTESIAN_POINT ( 'NONE',  ( -3.379380450443691952, -10.24275229525297348, 2.854909362179569587 ) ) ;
#1934 = ORIENTED_EDGE ( 'NONE', *, *, #19670, .T. ) ;
#1935 = CARTESIAN_POINT ( 'NONE',  ( -12.62966097655984754, -19.26462068372267566, 4.756751955311774083 ) ) ;
#1936 = CARTESIAN_POINT ( 'NONE',  ( -6.527808582316795949, -22.97900456129165647, 3.964901035250747885 ) ) ;
#1937 = EDGE_CURVE ( 'NONE', #14589, #15962, #18431, .T. ) ;
#1938 = CARTESIAN_POINT ( 'NONE',  ( -8.597191417683177406, -22.77556120703057729, 5.229004561291655584 ) ) ;
#1939 = VERTEX_POINT ( 'NONE', #10579 ) ;
#1940 = CARTESIAN_POINT ( 'NONE',  ( 13.84501469867711698, 4.235742283194553259, 4.791666666666684726 ) ) ;
#1941 = DIRECTION ( 'NONE',  ( -0.000000000000000000, -0.8660254037844364872, -0.5000000000000036637 ) ) ;
#1942 = VERTEX_POINT ( 'NONE', #10685 ) ;
#1943 = ORIENTED_EDGE ( 'NONE', *, *, #17724, .F. ) ;
#1944 = PLANE ( 'NONE',  #19092 ) ;
#1945 = VECTOR ( 'NONE', #14818, 1000.000000000000000 ) ;
#1946 = ORIENTED_EDGE ( 'NONE', *, *, #12802, .F. ) ;
#1947 = DIRECTION ( 'NONE',  ( 1.000000000000000000, 0.000000000000000000, 0.000000000000000000 ) ) ;
#1948 = EDGE_CURVE ( 'NONE', #3754, #20490, #16945, .T. ) ;
#1949 = EDGE_CURVE ( 'NONE', #12873, #1137, #9012, .T. ) ;
#1950 = VECTOR ( 'NONE', #12612, 1000.000000000000000 ) ;
#1951 = ORIENTED_EDGE ( 'NONE', *, *, #5701, .T. ) ;
#1952 = CARTESIAN_POINT ( 'NONE',  ( 6.159691417683176518, -22.67418626127524917, 1.729004561291651587 ) ) ;
#1953 = DIRECTION ( 'NONE',  ( 0.000000000000000000, 0.000000000000000000, 1.000000000000000000 ) ) ;
#1954 = CARTESIAN_POINT ( 'NONE',  ( -2.534747216115884161, -9.671180236796224960, 2.515503256513427210 ) ) ;
#1955 = CARTESIAN_POINT ( 'NONE',  ( 1.904508877737772998, -9.138371295333994837, 2.378667276417936627 ) ) ;
#1956 = CARTESIAN_POINT ( 'NONE',  ( -5.684058582316794173, -20.79840458871652942, 2.226721677130544030 ) ) ;
#1957 = VECTOR ( 'NONE', #11825, 1000.000000000000000 ) ;
#1958 = SURFACE_SIDE_STYLE ('',( #8035 ) ) ;
#1959 = CARTESIAN_POINT ( 'NONE',  ( 6.253441417683176518, -21.94931252712233061, 1.749999999999998446 ) ) ;
#1960 = DIRECTION ( 'NONE',  ( -0.000000000000000000, 0.000000000000000000, -1.000000000000000000 ) ) ;
#1961 = CARTESIAN_POINT ( 'NONE',  ( -10.65969141768317741, -22.36352608949543352, 2.479004561291652031 ) ) ;
#1962 = EDGE_CURVE ( 'NONE', #8181, #14649, #15384, .T. ) ;
#1963 = ORIENTED_EDGE ( 'NONE', *, *, #12166, .T. ) ;
#1964 = CARTESIAN_POINT ( 'NONE',  ( 9.527808582316795949, -24.47900456129166358, 4.586221378810390270 ) ) ;
#1965 = CARTESIAN_POINT ( 'NONE',  ( 13.06655316810189227, 2.048434989138931961, 5.965524842914772030 ) ) ;
#1966 = CARTESIAN_POINT ( 'NONE',  ( -13.11824772738305356, 3.909010232842670796, 6.755569162489314827 ) ) ;
#1967 = ORIENTED_EDGE ( 'NONE', *, *, #10492, .T. ) ;
#1968 = CARTESIAN_POINT ( 'NONE',  ( -20.00000000000000000, 3.499999999999999556, 1.500000000000000000 ) ) ;
#1969 = CARTESIAN_POINT ( 'NONE',  ( 0.000000000000000000, 16.00000000000000000, 1.000000000000000000 ) ) ;
#1970 = EDGE_LOOP ( 'NONE', ( #4283, #1261, #13717, #9024 ) ) ;
#1971 = VECTOR ( 'NONE', #1318, 1000.000000000000000 ) ;
#1972 = SHAPE_DEFINITION_REPRESENTATION ( #7841, #1880 ) ;
#1973 = ORIENTED_EDGE ( 'NONE', *, *, #18654, .F. ) ;
#1974 = AXIS2_PLACEMENT_3D ( 'NONE', #12021, #11711, #18107 ) ;
#1975 = CARTESIAN_POINT ( 'NONE',  ( 13.30678549240874275, -20.03395411350983935, 3.458247869257524254 ) ) ;
#1976 = ORIENTED_EDGE ( 'NONE', *, *, #18365, .F. ) ;
#1977 = EDGE_CURVE ( 'NONE', #7180, #17356, #1067, .T. ) ;
#1978 = CARTESIAN_POINT ( 'NONE',  ( -5.000000000000000000, -7.500000000000000000, 3.160254037844365094 ) ) ;
#1979 = DIRECTION ( 'NONE',  ( -0.000000000000000000, -0.000000000000000000, -1.000000000000000000 ) ) ;
#1980 = DIRECTION ( 'NONE',  ( 0.000000000000000000, 0.000000000000000000, -1.000000000000000000 ) ) ;
#1981 = CARTESIAN_POINT ( 'NONE',  ( 12.62500000000001954, -20.25000000000274269, 4.083333333315724012 ) ) ;
#1982 = DIRECTION ( 'NONE',  ( -0.000000000000000000, -0.000000000000000000, -1.000000000000000000 ) ) ;
#1983 = CARTESIAN_POINT ( 'NONE',  ( -13.37515323800563039, -20.24226148071262799, 4.627790572011877934 ) ) ;
#1984 = VECTOR ( 'NONE', #19824, 1000.000000000000000 ) ;
#1985 = CARTESIAN_POINT ( 'NONE',  ( 11.40280858231679595, -23.08622137881038938, 1.020995438708339309 ) ) ;
#1986 = CARTESIAN_POINT ( 'NONE',  ( -12.92761177809936513, -5.718105205959081339, 6.548537912490751900 ) ) ;
#1987 = CARTESIAN_POINT ( 'NONE',  ( -4.840308582316795061, -22.98484643305508612, 6.020995438708344416 ) ) ;
#1988 = EDGE_CURVE ( 'NONE', #15008, #14162, #18744, .T. ) ;
#1989 = AXIS2_PLACEMENT_3D ( 'NONE', #16860, #18234, #9127 ) ;
#1990 = EDGE_CURVE ( 'NONE', #13564, #6014, #16746, .T. ) ;
#1991 = DIRECTION ( 'NONE',  ( 1.000000000000000000, 0.000000000000000000, 0.000000000000000000 ) ) ;
#1992 = CARTESIAN_POINT ( 'NONE',  ( 23.31633994409548549, 10.00000000000000000, 1.000000000000000000 ) ) ;
#1993 = CARTESIAN_POINT ( 'NONE',  ( 9.434058582316795949, -22.67126532539354855, 4.242948236979545484 ) ) ;
#1994 = CARTESIAN_POINT ( 'NONE',  ( -9.253441417683177406, -21.94931252712233061, 1.749999999999998446 ) ) ;
#1995 = EDGE_LOOP ( 'NONE', ( #14834, #2151, #15596, #189, #1557, #14199, #4129, #1695 ) ) ;
#1996 = ORIENTED_EDGE ( 'NONE', *, *, #15355, .T. ) ;
#1997 = CARTESIAN_POINT ( 'NONE',  ( 13.38800411018677572, -19.59329243556743805, 5.436267741224407146 ) ) ;
#1998 = DIRECTION ( 'NONE',  ( -0.000000000000000000, -0.000000000000000000, -1.000000000000000000 ) ) ;
#1999 = ORIENTED_EDGE ( 'NONE', *, *, #17117, .T. ) ;
#2000 = DIRECTION ( 'NONE',  ( -0.000000000000000000, -0.000000000000000000, -1.000000000000000000 ) ) ;
#2001 = VECTOR ( 'NONE', #4648, 1000.000000000000000 ) ;
#2002 = PLANE ( 'NONE',  #13039 ) ;
#2003 = ADVANCED_FACE ( 'NONE', ( #10479 ), #2417, .T. ) ;
#2004 = CARTESIAN_POINT ( 'NONE',  ( 13.84264281492353987, 3.365962153638767607, 5.979325532956542233 ) ) ;
#2005 = STYLED_ITEM ( 'NONE', ( #4286 ), #15532 ) ;
#2006 = PRODUCT_DEFINITION_SHAPE ( 'NONE', 'NONE',  #20327 ) ;
#2007 = LINE ( 'NONE', #1419, #18889 ) ;
#2008 = CARTESIAN_POINT ( 'NONE',  ( 1.337453470010121714, -8.364917468222230923, 2.372643865078341019 ) ) ;
#2009 = VECTOR ( 'NONE', #12857, 1000.000000000000000 ) ;
#2010 = CARTESIAN_POINT ( 'NONE',  ( 1.126276606324276619, -9.114917468222230923, 1.622643865078341463 ) ) ;
#2011 = CARTESIAN_POINT ( 'NONE',  ( -13.10431844137356627, 3.955581289335645234, 6.006545679920360925 ) ) ;
#2012 = CARTESIAN_POINT ( 'NONE',  ( 8.309058582316792396, -23.27327832286945153, 2.298404588716537411 ) ) ;
#2013 = FACE_BOUND ( 'NONE', #12922, .T. ) ;
#2014 = CARTESIAN_POINT ( 'NONE',  ( 12.63249216759192350, -19.87164553660301536, 5.297612231341934041 ) ) ;
#2015 = CARTESIAN_POINT ( 'NONE',  ( -2.602174906157317835, -9.976397331638239052, 2.593889103792902606 ) ) ;
#2016 = AXIS2_PLACEMENT_3D ( 'NONE', #7727, #17954, #8239 ) ;
#2017 = PLANE ( 'NONE',  #19417 ) ;
#2018 = CARTESIAN_POINT ( 'NONE',  ( 7.753441417683176518, -21.94931252712233061, 1.749999999999998446 ) ) ;
#2019 = CARTESIAN_POINT ( 'NONE',  ( -8.590308582316797725, -21.63647391050454871, 2.479004561291657804 ) ) ;
#2020 = VERTEX_POINT ( 'NONE', #16848 ) ;
#2021 = CARTESIAN_POINT ( 'NONE',  ( 13.90439735423812273, 5.734566389025032684, 4.833333333333343695 ) ) ;
#2022 = CARTESIAN_POINT ( 'NONE',  ( 12.65051119073526564, -18.96168486786632457, 5.513701926248478102 ) ) ;
#2023 = CARTESIAN_POINT ( 'NONE',  ( 0.000000000000000000, 4.999999999999999112, 0.000000000000000000 ) ) ;
#2024 = ORIENTED_EDGE ( 'NONE', *, *, #17592, .T. ) ;
#2025 = VECTOR ( 'NONE', #946, 1000.000000000000000 ) ;
#2026 = EDGE_LOOP ( 'NONE', ( #6998, #5862, #6381, #5854 ) ) ;
#2027 = CARTESIAN_POINT ( 'NONE',  ( -4.999999999999998224, 0.000000000000000000, 9.999999999999998224 ) ) ;
#2028 = ADVANCED_FACE ( 'NONE', ( #9519 ), #15997, .T. ) ;
#2029 = LINE ( 'NONE', #8418, #8249 ) ;
#2030 = DIRECTION ( 'NONE',  ( 4.625929269271477434E-15, 1.000000000000000000, 0.000000000000000000 ) ) ;
#2031 = CARTESIAN_POINT ( 'NONE',  ( -26.19203811574920593, 0.000000000000000000, 1.000000000000000000 ) ) ;
#2032 = CARTESIAN_POINT ( 'NONE',  ( 2.340131407102140848, -12.21153219924485889, 2.225301406344140531 ) ) ;
#2033 = CARTESIAN_POINT ( 'NONE',  ( -11.99999999999999467, -17.50000000000000000, 1.000000000000000000 ) ) ;
#2034 = VECTOR ( 'NONE', #3246, 1000.000000000000000 ) ;
#2035 = CARTESIAN_POINT ( 'NONE',  ( 20.00000000000000000, -5.999999999999994671, 2.000000000000000000 ) ) ;
#2036 =( GEOMETRIC_REPRESENTATION_CONTEXT ( 3 ) GLOBAL_UNCERTAINTY_ASSIGNED_CONTEXT ( ( #2529 ) ) GLOBAL_UNIT_ASSIGNED_CONTEXT ( ( #17942, #5282, #9892 ) ) REPRESENTATION_CONTEXT ( 'NONE', 'WORKASPACE' ) );
#2037 = VECTOR ( 'NONE', #17601, 1000.000000000000000 ) ;
#2038 = CARTESIAN_POINT ( 'NONE',  ( 13.25854700851012424, -20.52162993467030461, 3.464734827531053440 ) ) ;
#2039 = CARTESIAN_POINT ( 'NONE',  ( -2.534747216115884161, -9.671180236796224960, 2.515503256513427210 ) ) ;
#2040 = CARTESIAN_POINT ( 'NONE',  ( -7.277808582316794173, -20.27099543870833642, 2.724438792969431589 ) ) ;
#2041 = VECTOR ( 'NONE', #4095, 1000.000000000000000 ) ;
#2042 = VECTOR ( 'NONE', #5090, 1000.000000000000000 ) ;
#2043 = CARTESIAN_POINT ( 'NONE',  ( 0.000000000000000000, -8.364917468222230923, 2.372643865078341019 ) ) ;
#2044 = EDGE_LOOP ( 'NONE', ( #18781, #8487, #12413, #10334 ) ) ;
#2045 = AXIS2_PLACEMENT_3D ( 'NONE', #5376, #13213, #11549 ) ;
#2046 = CARTESIAN_POINT ( 'NONE',  ( -12.62500797102436678, -19.49959746326937093, 4.516621614626514791 ) ) ;
#2047 = CARTESIAN_POINT ( 'NONE',  ( -6.809058582316794173, -23.27327832286945153, 2.298404588716537411 ) ) ;
#2048 = CARTESIAN_POINT ( 'NONE',  ( -6.815941417683176518, -20.79840458871654363, 4.773278322869464851 ) ) ;
#2049 = ORIENTED_EDGE ( 'NONE', *, *, #17282, .T. ) ;
#2050 = CARTESIAN_POINT ( 'NONE',  ( 13.39888564296547635, -18.29377503024027263, 4.763499963382565205 ) ) ;
#2051 = CARTESIAN_POINT ( 'NONE',  ( 8.119520639128047890, 9.000000000000001776, 0.000000000000000000 ) ) ;
#2052 = VERTEX_POINT ( 'NONE', #4816 ) ;
#2053 = ORIENTED_EDGE ( 'NONE', *, *, #13953, .F. ) ;
#2054 = DIRECTION ( 'NONE',  ( -1.000000000000000000, -0.000000000000000000, -0.000000000000000000 ) ) ;
#2055 = ORIENTED_EDGE ( 'NONE', *, *, #2145, .T. ) ;
#2056 = LINE ( 'NONE', #2458, #2757 ) ;
#2057 = VECTOR ( 'NONE', #20111, 1000.000000000000000 ) ;
#2058 = ORIENTED_EDGE ( 'NONE', *, *, #18139, .F. ) ;
#2059 = CARTESIAN_POINT ( 'NONE',  ( 5.878441417683177406, -23.74999999999999645, 3.449312527122335492 ) ) ;
#2060 = DIRECTION ( 'NONE',  ( -0.000000000000000000, -0.000000000000000000, -1.000000000000000000 ) ) ;
#2061 = EDGE_CURVE ( 'NONE', #12082, #18231, #10892, .T. ) ;
#2062 = CARTESIAN_POINT ( 'NONE',  ( 7.500000000000000000, -19.49999999999999645, 4.000000000000000000 ) ) ;
#2063 = LINE ( 'NONE', #18067, #12664 ) ;
#2064 = DIRECTION ( 'NONE',  ( 1.000000000000000000, 0.000000000000000000, 0.000000000000000000 ) ) ;
#2065 = DIRECTION ( 'NONE',  ( 0.000000000000000000, -0.000000000000000000, 1.000000000000000000 ) ) ;
#2066 = EDGE_CURVE ( 'NONE', #16093, #15361, #20622, .T. ) ;
#2067 = CARTESIAN_POINT ( 'NONE',  ( 11.87844141768317563, -23.74999999999999645, 3.449312527122335492 ) ) ;
#2068 = CARTESIAN_POINT ( 'NONE',  ( -13.81494360078803396, 11.64110105645932691, 10.00000000000000000 ) ) ;
#2069 = CARTESIAN_POINT ( 'NONE',  ( -5.690941417683176518, -23.27327832286946219, 4.701595411283453707 ) ) ;
#2070 = AXIS2_PLACEMENT_3D ( 'NONE', #12017, #835, #5643 ) ;
#2071 = CARTESIAN_POINT ( 'NONE',  ( -7.371558582316795949, -19.49999999999998934, 3.449312527122348371 ) ) ;
#2072 = VERTEX_POINT ( 'NONE', #9424 ) ;
#2073 = CARTESIAN_POINT ( 'NONE',  ( 12.63249216759192350, -19.87164553660301536, 5.297612231341934041 ) ) ;
#2074 = CARTESIAN_POINT ( 'NONE',  ( -12.62500000000001954, -20.25000000000274269, 4.083333333315724012 ) ) ;
#2075 = VERTEX_POINT ( 'NONE', #14428 ) ;
#2076 = DIRECTION ( 'NONE',  ( -1.000000000000000000, 0.000000000000000000, 0.000000000000000000 ) ) ;
#2077 = DIRECTION ( 'NONE',  ( 0.000000000000000000, 0.000000000000000000, 1.000000000000000000 ) ) ;
#2078 = ORIENTED_EDGE ( 'NONE', *, *, #18843, .T. ) ;
#2079 = DIRECTION ( 'NONE',  ( 0.000000000000000000, 0.000000000000000000, 1.000000000000000000 ) ) ;
#2080 = ORIENTED_EDGE ( 'NONE', *, *, #9533, .T. ) ;
#2081 = CARTESIAN_POINT ( 'NONE',  ( 12.74155597218489078, -19.97827208673946231, 3.535251045670558145 ) ) ;
#2082 = ORIENTED_EDGE ( 'NONE', *, *, #12798, .F. ) ;
#2083 = CARTESIAN_POINT ( 'NONE',  ( 15.86404127825609400, 4.999999999999999112, 1.000000000000000000 ) ) ;
#2084 = AXIS2_PLACEMENT_3D ( 'NONE', #16790, #18162, #16482 ) ;
#2085 = DIRECTION ( 'NONE',  ( 1.000000000000000000, 0.000000000000000000, 0.000000000000000000 ) ) ;
#2086 = EDGE_CURVE ( 'NONE', #19354, #13385, #1676, .T. ) ;
#2087 = CARTESIAN_POINT ( 'NONE',  ( 0.000000000000000000, 0.000000000000000000, 1.000000000000000000 ) ) ;
#2088 = CARTESIAN_POINT ( 'NONE',  ( 12.62745083560477966, -20.12623280195927933, 5.001038150054709419 ) ) ;
#2089 = DIRECTION ( 'NONE',  ( -1.000000000000000000, -0.000000000000000000, -0.000000000000000000 ) ) ;
#2090 = CARTESIAN_POINT ( 'NONE',  ( 7.277808582316795061, -19.52099543870833642, 2.413778621189609286 ) ) ;
#2091 = VECTOR ( 'NONE', #8690, 1000.000000000000000 ) ;
#2092 = CARTESIAN_POINT ( 'NONE',  ( -13.10026320386584153, 3.000791795219782454, 6.736037912489353019 ) ) ;
#2093 = CARTESIAN_POINT ( 'NONE',  ( -10.47219141768317741, -24.47900456129165292, 2.413778621189595963 ) ) ;
#2094 = DIRECTION ( 'NONE',  ( 0.000000000000000000, 0.000000000000000000, -1.000000000000000000 ) ) ;
#2095 = FACE_OUTER_BOUND ( 'NONE', #234, .T. ) ;
#2096 = VECTOR ( 'NONE', #14954, 1000.000000000000000 ) ;
#2097 = CARTESIAN_POINT ( 'NONE',  ( 9.621558582316795949, -22.99999999999999645, 3.550687472877652073 ) ) ;
#2098 = CARTESIAN_POINT ( 'NONE',  ( -4.003441417683176518, -22.05068747287765873, 5.250000000000000888 ) ) ;
#2099 = ORIENTED_EDGE ( 'NONE', *, *, #338, .F. ) ;
#2100 = ORIENTED_EDGE ( 'NONE', *, *, #7749, .T. ) ;
#2101 = CARTESIAN_POINT ( 'NONE',  ( 13.39359219590679295, -19.31109410670777038, 5.491647114909025795 ) ) ;
#2102 = CARTESIAN_POINT ( 'NONE',  ( -11.00000000000000000, -23.83493649053891517, 4.999999999999999112 ) ) ;
#2103 = ORIENTED_EDGE ( 'NONE', *, *, #19635, .T. ) ;
#2104 = DIRECTION ( 'NONE',  ( 0.000000000000000000, -0.9659258262890672020, 0.2588190451025245142 ) ) ;
#2105 = DIRECTION ( 'NONE',  ( 0.000000000000000000, -1.000000000000000000, 0.000000000000000000 ) ) ;
#2106 = CARTESIAN_POINT ( 'NONE',  ( -9.305650798910056309, 9.000000000000001776, 0.000000000000000000 ) ) ;
#2107 = CARTESIAN_POINT ( 'NONE',  ( 13.38921792038197900, -19.53199502070850357, 5.456033026503027017 ) ) ;
#2108 = ADVANCED_FACE ( 'NONE', ( #17469 ), #1571, .F. ) ;
#2109 = EDGE_CURVE ( 'NONE', #13777, #3840, #4508, .T. ) ;
#2110 = LINE ( 'NONE', #640, #1184 ) ;
#2111 = CARTESIAN_POINT ( 'NONE',  ( 2.910499702382182807, -8.879427762644468203, 2.504780387061739333 ) ) ;
#2112 = AXIS2_PLACEMENT_3D ( 'NONE', #10886, #2929, #12639 ) ;
#2113 = DIRECTION ( 'NONE',  ( 0.000000000000000000, 1.000000000000000000, -0.000000000000000000 ) ) ;
#2114 = CARTESIAN_POINT ( 'NONE',  ( -12.82182472306881671, -9.560351485048736109, 4.965845106672846399 ) ) ;
#2115 = CARTESIAN_POINT ( 'NONE',  ( 6.246558582316794173, -21.94931252712234482, 5.250000000000000888 ) ) ;
#2116 = CARTESIAN_POINT ( 'NONE',  ( -14.49999999999998579, -21.99999999999999645, 11.68378559369222280 ) ) ;
#2117 = CARTESIAN_POINT ( 'NONE',  ( 13.10756170493883310, 4.119366099410778581, 6.001761809183453700 ) ) ;
#2118 = CARTESIAN_POINT ( 'NONE',  ( -2.559937518207947793, -9.746075135043517079, 2.534737762559237773 ) ) ;
#2119 = CARTESIAN_POINT ( 'NONE',  ( 7.090308582316795061, -21.63647391050454871, 2.479004561291657804 ) ) ;
#2120 = CARTESIAN_POINT ( 'NONE',  ( 12.06594141768317563, -23.20159541128344927, 2.226721677130534705 ) ) ;
#2121 = VECTOR ( 'NONE', #12009, 1000.000000000000000 ) ;
#2122 = CARTESIAN_POINT ( 'NONE',  ( -6.246558582316795949, -21.94931252712234127, 4.499999999999999112 ) ) ;
#2123 = ORIENTED_EDGE ( 'NONE', *, *, #13146, .T. ) ;
#2124 = CARTESIAN_POINT ( 'NONE',  ( 13.10026320386584153, 3.000791795219782454, 6.736037912489353019 ) ) ;
#2125 = CARTESIAN_POINT ( 'NONE',  ( 12.62515856830665584, -19.49199230051052822, 4.565864671500353467 ) ) ;
#2126 = CARTESIAN_POINT ( 'NONE',  ( -12.66618699081223198, -20.05307589586896455, 3.545538277555074114 ) ) ;
#2127 = VERTEX_POINT ( 'NONE', #9728 ) ;
#2128 = ORIENTED_EDGE ( 'NONE', *, *, #1216, .F. ) ;
#2129 = CARTESIAN_POINT ( 'NONE',  ( -27.50000000000000711, 4.999999999999999112, 0.000000000000000000 ) ) ;
#2130 = PLANE ( 'NONE',  #19291 ) ;
#2131 = ADVANCED_FACE ( 'NONE', ( #17256 ), #11193, .T. ) ;
#2132 = EDGE_CURVE ( 'NONE', #15823, #3062, #2935, .T. ) ;
#2133 = DIRECTION ( 'NONE',  ( -1.000000000000000000, 0.000000000000000000, 0.000000000000000000 ) ) ;
#2134 = PLANE ( 'NONE',  #13664 ) ;
#2135 = CARTESIAN_POINT ( 'NONE',  ( 1.707060460004204527, -9.864918773552613374, 2.372644200313257290 ) ) ;
#2136 = CARTESIAN_POINT ( 'NONE',  ( 7.499999999999999112, -19.49999999999999645, 4.000000000000000000 ) ) ;
#2137 = DIRECTION ( 'NONE',  ( 1.000000000000000000, 0.000000000000000000, -0.000000000000000000 ) ) ;
#2138 = LINE ( 'NONE', #19928, #17039 ) ;
#2139 = DIRECTION ( 'NONE',  ( 0.000000000000000000, -1.000000000000000000, 0.000000000000000000 ) ) ;
#2140 = CARTESIAN_POINT ( 'NONE',  ( -8.027808582316792396, -23.72900456129165647, 4.275561207030568411 ) ) ;
#2141 = CARTESIAN_POINT ( 'NONE',  ( -2.445888733774860935, -8.532121313016713060, 2.415585152653916712 ) ) ;
#2142 = EDGE_LOOP ( 'NONE', ( #17794, #16886, #15579, #5598 ) ) ;
#2143 = CARTESIAN_POINT ( 'NONE',  ( -13.38090111944825367, -19.20199346786276351, 4.743968713382380464 ) ) ;
#2144 = CARTESIAN_POINT ( 'NONE',  ( -5.215308582316793284, -23.77099543870833998, 2.825813738724734847 ) ) ;
#2145 = EDGE_CURVE ( 'NONE', #15521, #3725, #3146, .T. ) ;
#2146 = CARTESIAN_POINT ( 'NONE',  ( -10.09719141768317741, -22.77556120703057729, 5.229004561291655584 ) ) ;
#2147 = ORIENTED_EDGE ( 'NONE', *, *, #7241, .F. ) ;
#2148 = CARTESIAN_POINT ( 'NONE',  ( 13.84501469867711698, 4.235742283194553259, 4.166666666666765551 ) ) ;
#2149 = LINE ( 'NONE', #8531, #12053 ) ;
#2150 = ORIENTED_EDGE ( 'NONE', *, *, #4677, .T. ) ;
#2151 = ORIENTED_EDGE ( 'NONE', *, *, #18217, .T. ) ;
#2152 = LINE ( 'NONE', #11255, #11386 ) ;
#2153 = ORIENTED_EDGE ( 'NONE', *, *, #2460, .F. ) ;
#2154 = CARTESIAN_POINT ( 'NONE',  ( -13.37499999999995026, -20.24999999999991829, 3.465895369911768054 ) ) ;
#2155 = ORIENTED_EDGE ( 'NONE', *, *, #8173, .T. ) ;
#2156 = CARTESIAN_POINT ( 'NONE',  ( 3.974842109207561425, -21.82955800590261930, 5.256404853634145447 ) ) ;
#2157 = CYLINDRICAL_SURFACE ( 'NONE', #20022, 2.500000000000000444 ) ;
#2158 = CARTESIAN_POINT ( 'NONE',  ( 4.000000000000000000, -12.50000000000000000, 3.464723819589916154 ) ) ;
#2159 = CARTESIAN_POINT ( 'NONE',  ( 2.817596665886821672, -11.50588678273290988, 2.986692549455723267 ) ) ;
#2160 = DIRECTION ( 'NONE',  ( -1.000000000000000000, -3.469446951953611033E-15, 0.000000000000000000 ) ) ;
#2161 = CARTESIAN_POINT ( 'NONE',  ( 12.62500028073152869, -20.99998582305707728, 4.544498183892649479 ) ) ;
#2162 = LINE ( 'NONE', #2370, #7636 ) ;
#2163 = CARTESIAN_POINT ( 'NONE',  ( 10.65969141768318096, -22.67418626127524917, 1.729004561291651809 ) ) ;
#2164 = CARTESIAN_POINT ( 'NONE',  ( 0.000000000000000000, 9.000000000000001776, 1.000000000000000000 ) ) ;
#2165 = CARTESIAN_POINT ( 'NONE',  ( -5.315941417683176518, -21.32873467460645145, 4.242948236979555254 ) ) ;
#2166 = CARTESIAN_POINT ( 'NONE',  ( -11.12155858231679595, -24.50000000000000000, 3.550687472877651629 ) ) ;
#2167 = ORIENTED_EDGE ( 'NONE', *, *, #14644, .T. ) ;
#2168 = CARTESIAN_POINT ( 'NONE',  ( 12.62500000000001954, -20.25000000000274269, 4.083333333315724012 ) ) ;
#2169 = CARTESIAN_POINT ( 'NONE',  ( -13.11465082267961968, 3.727366545318180791, 6.751662912489328150 ) ) ;
#2170 = VERTEX_POINT ( 'NONE', #17570 ) ;
#2171 = EDGE_CURVE ( 'NONE', #5966, #15986, #11290, .T. ) ;
#2172 = DIRECTION ( 'NONE',  ( -0.000000000000000000, 0.000000000000000000, -1.000000000000000000 ) ) ;
#2173 = PLANE ( 'NONE',  #15347 ) ;
#2174 = ORIENTED_EDGE ( 'NONE', *, *, #4992, .T. ) ;
#2175 = ORIENTED_EDGE ( 'NONE', *, *, #4062, .T. ) ;
#2176 = DIRECTION ( 'NONE',  ( -0.000000000000000000, -1.000000000000000000, 0.000000000000000000 ) ) ;
#2177 = AXIS2_PLACEMENT_3D ( 'NONE', #14012, #18844, #20307 ) ;
#2178 = CIRCLE ( 'NONE', #12865, 1.000000000000002665 ) ;
#2179 = ORIENTED_EDGE ( 'NONE', *, *, #14452, .F. ) ;
#2180 = CARTESIAN_POINT ( 'NONE',  ( -5.999999999999999112, -7.500000000000047073, 9.999999999999998224 ) ) ;
#2181 = CARTESIAN_POINT ( 'NONE',  ( 13.11740841389447709, 4.616624901677048420, 5.813473370769506765 ) ) ;
#2182 = CARTESIAN_POINT ( 'NONE',  ( -1.126276606324276619, -8.364917468222230923, 1.622643865078341907 ) ) ;
#2183 = DIRECTION ( 'NONE',  ( 0.000000000000000000, 0.000000000000000000, 1.000000000000000000 ) ) ;
#2184 = CARTESIAN_POINT ( 'NONE',  ( -0.000000000000000000, 11.64110105645932691, 0.000000000000000000 ) ) ;
#2185 = CARTESIAN_POINT ( 'NONE',  ( 12.72125031657057015, -15.38935901321805133, 5.590524842915047365 ) ) ;
#2186 = CARTESIAN_POINT ( 'NONE',  ( -14.49999999999998579, -21.99999999999999645, 11.00000000000000178 ) ) ;
#2187 = CARTESIAN_POINT ( 'NONE',  ( 11.12155858231679595, -24.50000000000000000, 3.550687472877651629 ) ) ;
#2188 = CARTESIAN_POINT ( 'NONE',  ( -12.96597876160390683, -3.780572539034193102, 6.590204579154564257 ) ) ;
#2189 = CARTESIAN_POINT ( 'NONE',  ( -4.472191417683178294, -24.47900456129165292, 2.413778621189595963 ) ) ;
#2190 = LINE ( 'NONE', #10147, #4721 ) ;
#2191 = CARTESIAN_POINT ( 'NONE',  ( -0.1250000000000001110, 0.000000000000000000, 1.000000000000000000 ) ) ;
#2192 = AXIS2_PLACEMENT_3D ( 'NONE', #8146, #6982, #8958 ) ;
#2193 = EDGE_CURVE ( 'NONE', #7935, #12082, #20718, .T. ) ;
#2194 = CARTESIAN_POINT ( 'NONE',  ( 6.809058582316796837, -22.74294823697954016, 2.828734674606448785 ) ) ;
#2195 = CARTESIAN_POINT ( 'NONE',  ( 12.00000000000000178, -18.50000000000000355, 1.000000000000000000 ) ) ;
#2196 = ORIENTED_EDGE ( 'NONE', *, *, #19330, .T. ) ;
#2197 = ORIENTED_EDGE ( 'NONE', *, *, #13364, .T. ) ;
#2198 = CARTESIAN_POINT ( 'NONE',  ( 13.85980676119184629, 4.232741440188380722, 5.965367510457697975 ) ) ;
#2199 = LINE ( 'NONE', #6712, #16115 ) ;
#2200 =( LENGTH_UNIT ( ) NAMED_UNIT ( * ) SI_UNIT ( .MILLI., .METRE. ) );
#2201 = ORIENTED_EDGE ( 'NONE', *, *, #2707, .T. ) ;
#2202 = CARTESIAN_POINT ( 'NONE',  ( -14.49999999999999645, -22.99999999999998579, 4.000000000000000000 ) ) ;
#2203 = EDGE_CURVE ( 'NONE', #17464, #10229, #7754, .T. ) ;
#2204 = EDGE_CURVE ( 'NONE', #3058, #16093, #14214, .T. ) ;
#2205 = DIRECTION ( 'NONE',  ( 0.000000000000000000, 0.000000000000000000, 1.000000000000000000 ) ) ;
#2206 = DIRECTION ( 'NONE',  ( -0.000000000000000000, -0.000000000000000000, -1.000000000000000000 ) ) ;
#2207 = CARTESIAN_POINT ( 'NONE',  ( 13.38450946332969771, -19.76977210184853462, 5.359796180098093998 ) ) ;
#2208 = CARTESIAN_POINT ( 'NONE',  ( 11.00000000000000000, -20.16506350946107418, 5.250000000000000000 ) ) ;
#2209 = CARTESIAN_POINT ( 'NONE',  ( 0.5631383031621635116, -8.364917468222230923, 2.372643865078341019 ) ) ;
#2210 = LINE ( 'NONE', #8592, #5043 ) ;
#2211 = CARTESIAN_POINT ( 'NONE',  ( -13.12529380813666435, 5.014837310896125722, 5.033295791462342628 ) ) ;
#2212 = CARTESIAN_POINT ( 'NONE',  ( 6.621558582316794173, -23.74999999999999645, 3.550687472877651629 ) ) ;
#2213 = DIRECTION ( 'NONE',  ( 1.000000000000000000, -0.000000000000000000, 0.000000000000000000 ) ) ;
#2214 = CARTESIAN_POINT ( 'NONE',  ( 12.63465172146706728, -19.76258806590802664, 5.372658420469845986 ) ) ;
#2215 = CARTESIAN_POINT ( 'NONE',  ( -3.162271481458107658, -13.95306990448253437, 3.615178062515473911 ) ) ;
#2216 = CARTESIAN_POINT ( 'NONE',  ( 11.30905858231679595, -22.74294823697954016, 2.828734674606448785 ) ) ;
#2217 = EDGE_CURVE ( 'NONE', #16327, #17198, #9616, .T. ) ;
#2218 = CARTESIAN_POINT ( 'NONE',  ( 9.440941417683177406, -20.72672167713052715, 2.298404588716546293 ) ) ;
#2219 = CARTESIAN_POINT ( 'NONE',  ( -11.12155858231679417, -23.74999999999999645, 3.550687472877651629 ) ) ;
#2220 = ORIENTED_EDGE ( 'NONE', *, *, #13815, .T. ) ;
#2221 = CARTESIAN_POINT ( 'NONE',  ( 12.65346245025441263, -19.56264626215117275, 6.228892365149262922 ) ) ;
#2222 = CARTESIAN_POINT ( 'NONE',  ( 12.62499999999998224, -19.49999999999991473, 4.333333333333343695 ) ) ;
#2223 = VECTOR ( 'NONE', #15836, 1000.000000000000000 ) ;
#2224 = FACE_OUTER_BOUND ( 'NONE', #1017, .T. ) ;
#2225 = EDGE_LOOP ( 'NONE', ( #1668, #20220, #7372, #9771, #20404 ) ) ;
#2226 = VERTEX_POINT ( 'NONE', #110 ) ;
#2227 = DIRECTION ( 'NONE',  ( 0.000000000000000000, -1.000000000000000000, 0.000000000000000000 ) ) ;
#2228 = DIRECTION ( 'NONE',  ( 0.000000000000000000, -1.000000000000000000, 0.000000000000000000 ) ) ;
#2229 = DIRECTION ( 'NONE',  ( 1.000000000000000000, 0.000000000000000000, -0.000000000000000000 ) ) ;
#2230 = FACE_OUTER_BOUND ( 'NONE', #17720, .T. ) ;
#2231 = CARTESIAN_POINT ( 'NONE',  ( 2.583953725994688533, -9.847075946378776479, 2.560676788604062004 ) ) ;
#2232 = DIRECTION ( 'NONE',  ( 0.000000000000000000, -0.1264857625231113059, 0.9919684228235025047 ) ) ;
#2233 = DIRECTION ( 'NONE',  ( -0.000000000000000000, 0.000000000000000000, -1.000000000000000000 ) ) ;
#2234 = PLANE ( 'NONE',  #9369 ) ;
#2235 = LINE ( 'NONE', #6754, #14984 ) ;
#2236 = CARTESIAN_POINT ( 'NONE',  ( -6.621558582316794173, -23.74999999999999645, 3.550687472877651629 ) ) ;
#2237 = CARTESIAN_POINT ( 'NONE',  ( -2.910499702382182807, -8.879427762644468203, 2.504780387061739333 ) ) ;
#2238 = ORIENTED_EDGE ( 'NONE', *, *, #3662, .T. ) ;
#2239 = CARTESIAN_POINT ( 'NONE',  ( -13.09556065010287362, 4.263312830196960057, 5.034075356110313315 ) ) ;
#2240 = CARTESIAN_POINT ( 'NONE',  ( -9.340308582316794173, -22.67418626127525982, 5.270995438708342640 ) ) ;
#2241 = ADVANCED_FACE ( 'NONE', ( #18847 ), #6496, .T. ) ;
#2242 = CARTESIAN_POINT ( 'NONE',  ( -8.034691417683175629, -20.22900456129164581, 2.825813738724747726 ) ) ;
#2243 = ORIENTED_EDGE ( 'NONE', *, *, #4992, .F. ) ;
#2244 = EDGE_CURVE ( 'NONE', #10986, #14610, #12547, .T. ) ;
#2245 = CARTESIAN_POINT ( 'NONE',  ( 13.75871503850933841, -0.8723905552644914962, 5.888179699623941943 ) ) ;
#2246 = FACE_OUTER_BOUND ( 'NONE', #1920, .T. ) ;
#2247 = ORIENTED_EDGE ( 'NONE', *, *, #4115, .T. ) ;
#2248 = VERTEX_POINT ( 'NONE', #19053 ) ;
#2249 = CARTESIAN_POINT ( 'NONE',  ( -10.43924542913431175, 0.000000000000000000, 0.000000000000000000 ) ) ;
#2250 = ORIENTED_EDGE ( 'NONE', *, *, #19877, .T. ) ;
#2251 = CARTESIAN_POINT ( 'NONE',  ( -13.37499999999998224, -20.24999999999998934, 4.291666666666698937 ) ) ;
#2252 = EDGE_LOOP ( 'NONE', ( #11663, #6423, #14103, #14980 ) ) ;
#2253 = CARTESIAN_POINT ( 'NONE',  ( 7.378441417683176518, -23.74999999999999645, 3.449312527122335492 ) ) ;
#2254 = EDGE_CURVE ( 'NONE', #8019, #14361, #4710, .T. ) ;
#2255 = CARTESIAN_POINT ( 'NONE',  ( -11.00000000000000000, -20.16506350946107418, 5.000000000000000000 ) ) ;
#2256 = LINE ( 'NONE', #8448, #6316 ) ;
#2257 = CARTESIAN_POINT ( 'NONE',  ( 3.549867680106858714, -10.29705900472337632, 2.118856410057032402 ) ) ;
#2258 = CARTESIAN_POINT ( 'NONE',  ( -8.402808582316792396, -22.77556120703056308, 1.770995438708340197 ) ) ;
#2259 = CARTESIAN_POINT ( 'NONE',  ( 13.90439706815434739, 5.734551941788608609, 5.045486763335835789 ) ) ;
#2260 = CARTESIAN_POINT ( 'NONE',  ( -17.94064177244175795, 0.000000000000000000, 1.000000000000000000 ) ) ;
#2261 = CARTESIAN_POINT ( 'NONE',  ( 5.784691417683179182, -23.77099543870834353, 4.174186261275252718 ) ) ;
#2262 = CARTESIAN_POINT ( 'NONE',  ( -12.64571531779736979, -19.20387645123237164, 5.508493592915143289 ) ) ;
#2263 = CARTESIAN_POINT ( 'NONE',  ( -6.159691417683175629, -22.36352608949543352, 2.479004561291652031 ) ) ;
#2264 = CARTESIAN_POINT ( 'NONE',  ( -8.684058582316795949, -20.26807450282662160, 1.696391591240633101 ) ) ;
#2265 = ORIENTED_EDGE ( 'NONE', *, *, #16645, .F. ) ;
#2266 = CARTESIAN_POINT ( 'NONE',  ( 13.12424783836753228, 4.962015837561366993, 5.328858059679200565 ) ) ;
#2267 = CARTESIAN_POINT ( 'NONE',  ( -12.64387510712649565, -19.29680709011273976, 5.506486987317513737 ) ) ;
#2268 = ORIENTED_EDGE ( 'NONE', *, *, #2171, .F. ) ;
#2269 = VECTOR ( 'NONE', #502, 1000.000000000000000 ) ;
#2270 = PLANE ( 'NONE',  #1929 ) ;
#2271 = CYLINDRICAL_SURFACE ( 'NONE', #15677, 0.4999999999999987232 ) ;
#2272 = EDGE_LOOP ( 'NONE', ( #10405, #2024, #11415, #19506 ) ) ;
#2273 = ORIENTED_EDGE ( 'NONE', *, *, #15162, .F. ) ;
#2274 = CARTESIAN_POINT ( 'NONE',  ( 12.73854111515253607, -19.98117175391610090, 3.535666685490541639 ) ) ;
#2275 = ORIENTED_EDGE ( 'NONE', *, *, #1977, .F. ) ;
#2276 = FACE_OUTER_BOUND ( 'NONE', #13922, .T. ) ;
#2277 = ADVANCED_FACE ( 'NONE', ( #7005 ), #6698, .F. ) ;
#2278 = CARTESIAN_POINT ( 'NONE',  ( 12.95145221759166354, -3.764163011652346569, 5.840524842913703552 ) ) ;
#2279 = VECTOR ( 'NONE', #4991, 1000.000000000000000 ) ;
#2280 = CARTESIAN_POINT ( 'NONE',  ( -2.916276642307554123, -11.05036367517186058, 2.119705115445599475 ) ) ;
#2281 = DIRECTION ( 'NONE',  ( 0.000000000000000000, -0.000000000000000000, 1.000000000000000000 ) ) ;
#2282 = LINE ( 'NONE', #8672, #3826 ) ;
#2283 = DIRECTION ( 'NONE',  ( -1.000000000000000000, 0.000000000000000000, 0.000000000000000000 ) ) ;
#2284 = DIRECTION ( 'NONE',  ( 0.000000000000000000, 1.000000000000000000, -0.000000000000000000 ) ) ;
#2285 = CARTESIAN_POINT ( 'NONE',  ( 11.31594141768317741, -20.26807450282663225, 5.303608408759377113 ) ) ;
#2286 = CARTESIAN_POINT ( 'NONE',  ( -13.12526104302547836, 5.013182672784613381, 5.066812735559260261 ) ) ;
#2287 = CARTESIAN_POINT ( 'NONE',  ( -7.003441417683177406, -22.05068747287766229, 6.000000000000001776 ) ) ;
#2288 = VERTEX_POINT ( 'NONE', #6896 ) ;
#2289 = CARTESIAN_POINT ( 'NONE',  ( 10.84030858231679240, -22.67418626127525982, 5.270995438708342640 ) ) ;
#2290 = DIRECTION ( 'NONE',  ( 1.000000000000000000, 0.000000000000000000, 0.000000000000000000 ) ) ;
#2291 = CARTESIAN_POINT ( 'NONE',  ( -13.87470602645761986, 4.985154336109792972, 4.666666666666619889 ) ) ;
#2292 = VECTOR ( 'NONE', #11978, 1000.000000000000000 ) ;
#2293 = CARTESIAN_POINT ( 'NONE',  ( 8.121558582316795949, -22.99999999999999645, 3.550687472877652073 ) ) ;
#2294 = CARTESIAN_POINT ( 'NONE',  ( 21.17243175760212637, 9.000000000000001776, 1.000000000000000000 ) ) ;
#2295 = VECTOR ( 'NONE', #5825, 1000.000000000000000 ) ;
#2296 = VERTEX_POINT ( 'NONE', #5326 ) ;
#2297 = VERTEX_POINT ( 'NONE', #3653 ) ;
#2298 = CARTESIAN_POINT ( 'NONE',  ( 13.86470821076586368, 4.480264643675554659, 5.874551681240599343 ) ) ;
#2299 = CARTESIAN_POINT ( 'NONE',  ( -14.56494360078803396, 0.000000000000000000, 1.000000000000000000 ) ) ;
#2300 = ORIENTED_EDGE ( 'NONE', *, *, #12681, .T. ) ;
#2301 = CARTESIAN_POINT ( 'NONE',  ( -14.49999999999998579, -24.49999999999999289, 4.000000000000000000 ) ) ;
#2302 = DIRECTION ( 'NONE',  ( -0.000000000000000000, -0.000000000000000000, -1.000000000000000000 ) ) ;
#2303 = CARTESIAN_POINT ( 'NONE',  ( 24.50000000000000000, 0.000000000000000000, 1.000000000000000000 ) ) ;
#2304 = CARTESIAN_POINT ( 'NONE',  ( 13.37561105820882013, -20.21914156045197686, 4.753815841436231260 ) ) ;
#2305 = VECTOR ( 'NONE', #12289, 1000.000000000000000 ) ;
#2306 = LINE ( 'NONE', #5456, #3851 ) ;
#2307 = AXIS2_PLACEMENT_3D ( 'NONE', #13236, #11476, #5291 ) ;
#2308 = CARTESIAN_POINT ( 'NONE',  ( 3.379380450443691952, -10.24275229525297348, 2.854909362179569587 ) ) ;
#2309 = ADVANCED_FACE ( 'NONE', ( #9829 ), #11700, .T. ) ;
#2310 = AXIS2_PLACEMENT_3D ( 'NONE', #2824, #11084, #17041 ) ;
#2311 = LINE ( 'NONE', #16438, #17401 ) ;
#2312 = CARTESIAN_POINT ( 'NONE',  ( -12.62500004114794372, -19.49999792202770621, 4.520295319612473328 ) ) ;
#2313 = LINE ( 'NONE', #8402, #9725 ) ;
#2314 = CARTESIAN_POINT ( 'NONE',  ( 13.10624331898488037, 4.052787608736739600, 6.006964772046813117 ) ) ;
#2315 = CARTESIAN_POINT ( 'NONE',  ( -2.513306525444908512, -9.622685169956881168, 2.503048754562789746 ) ) ;
#2316 = EDGE_CURVE ( 'NONE', #7608, #1742, #18098, .T. ) ;
#2317 = CARTESIAN_POINT ( 'NONE',  ( 8.777808582316797725, -21.02099543870833998, 3.035098964749253003 ) ) ;
#2318 = EDGE_CURVE ( 'NONE', #1636, #2072, #14743, .T. ) ;
#2319 = CARTESIAN_POINT ( 'NONE',  ( 7.565941417683176518, -23.20159541128344927, 2.226721677130534705 ) ) ;
#2320 = CARTESIAN_POINT ( 'NONE',  ( -7.840308582316794173, -22.67418626127525982, 5.270995438708342640 ) ) ;
#2321 = ORIENTED_EDGE ( 'NONE', *, *, #8111, .F. ) ;
#2322 = CARTESIAN_POINT ( 'NONE',  ( 12.69740987707854707, -17.34330120752609616, 6.298537912489285517 ) ) ;
#2323 = CARTESIAN_POINT ( 'NONE',  ( 12.99447614883396973, -0.8414544838704021146, 5.153345106674984244 ) ) ;
#2324 = DIRECTION ( 'NONE',  ( 0.000000000000000000, 0.000000000000000000, -1.000000000000000000 ) ) ;
#2325 = ORIENTED_EDGE ( 'NONE', *, *, #19639, .F. ) ;
#2326 = UNCERTAINTY_MEASURE_WITH_UNIT (LENGTH_MEASURE( 1.000000000000000082E-05 ), #12848, 'distance_accuracy_value', 'NONE');
#2327 = VECTOR ( 'NONE', #18023, 1000.000000000000000 ) ;
#2328 = ORIENTED_EDGE ( 'NONE', *, *, #7251, .F. ) ;
#2329 = CARTESIAN_POINT ( 'NONE',  ( -20.92243175760212637, 9.000000000000001776, 0.000000000000000000 ) ) ;
#2330 = VECTOR ( 'NONE', #7851, 1000.000000000000000 ) ;
#2331 = CARTESIAN_POINT ( 'NONE',  ( -20.75349085826862350, 11.64110105645932691, 10.00000000000000000 ) ) ;
#2332 = CARTESIAN_POINT ( 'NONE',  ( -7.499999999999999112, -24.49999999999999289, 4.000000000000000000 ) ) ;
#2333 = EDGE_CURVE ( 'NONE', #2461, #7526, #5018, .T. ) ;
#2334 = CARTESIAN_POINT ( 'NONE',  ( 5.000000000000000000, -7.500000000000000000, 3.160254037844365094 ) ) ;
#2335 = CARTESIAN_POINT ( 'NONE',  ( 2.602174906157317835, -9.976397331638239052, 2.593889103792902606 ) ) ;
#2336 = DIRECTION ( 'NONE',  ( 0.000000000000000000, -1.000000000000000000, 0.000000000000000000 ) ) ;
#2337 = DIRECTION ( 'NONE',  ( -1.000000000000000000, 6.938893903907222067E-15, 0.000000000000000000 ) ) ;
#2338 = CARTESIAN_POINT ( 'NONE',  ( -26.19203811574920593, 11.64110105645932691, 0.000000000000000000 ) ) ;
#2339 = DIRECTION ( 'NONE',  ( 1.000000000000000000, 0.000000000000000000, 0.000000000000000000 ) ) ;
#2340 = CARTESIAN_POINT ( 'NONE',  ( -5.309058582316794173, -23.27327832286945153, 2.298404588716537411 ) ) ;
#2341 = CARTESIAN_POINT ( 'NONE',  ( -3.882031223148668886, -13.81156101447257889, 3.771450735391772557 ) ) ;
#2342 = ORIENTED_EDGE ( 'NONE', *, *, #2552, .T. ) ;
#2343 = CARTESIAN_POINT ( 'NONE',  ( -13.37559048950600626, -19.47018027994350220, 4.620717101209816491 ) ) ;
#2344 = CARTESIAN_POINT ( 'NONE',  ( -9.809058582316794173, -23.27327832286945153, 2.298404588716537411 ) ) ;
#2345 = AXIS2_PLACEMENT_3D ( 'NONE', #13280, #10258, #18214 ) ;
#2346 = CARTESIAN_POINT ( 'NONE',  ( 8.027808582316795949, -24.47900456129166358, 4.586221378810390270 ) ) ;
#2347 = CARTESIAN_POINT ( 'NONE',  ( -8.503441417683177406, -22.05068747287766229, 4.499999999999999112 ) ) ;
#2348 = ORIENTED_EDGE ( 'NONE', *, *, #6891, .F. ) ;
#2349 = CARTESIAN_POINT ( 'NONE',  ( 13.83544900551672185, 3.002674778589386140, 5.971513032956590195 ) ) ;
#2350 = DIRECTION ( 'NONE',  ( 1.000000000000000000, 0.000000000000000000, 0.000000000000000000 ) ) ;
#2351 = ORIENTED_EDGE ( 'NONE', *, *, #5064, .F. ) ;
#2352 = EDGE_CURVE ( 'NONE', #14282, #12772, #12019, .T. ) ;
#2353 = ORIENTED_EDGE ( 'NONE', *, *, #254, .F. ) ;
#2354 = CARTESIAN_POINT ( 'NONE',  ( -25.29469207716615031, 0.000000000000000000, 0.000000000000000000 ) ) ;
#2355 = ORIENTED_EDGE ( 'NONE', *, *, #20532, .T. ) ;
#2356 = CARTESIAN_POINT ( 'NONE',  ( -13.17791111847408025, 0.000000000000000000, 0.000000000000000000 ) ) ;
#2357 = EDGE_LOOP ( 'NONE', ( #4842, #13020, #8609, #10338 ) ) ;
#2358 = VECTOR ( 'NONE', #170, 1000.000000000000000 ) ;
#2359 = LINE ( 'NONE', #5401, #7994 ) ;
#2360 = DIRECTION ( 'NONE',  ( 0.000000000000000000, 0.2487476929738665354, 0.9685683172808094987 ) ) ;
#2361 = VECTOR ( 'NONE', #11432, 1000.000000000000000 ) ;
#2362 = EDGE_CURVE ( 'NONE', #12874, #9416, #3451, .T. ) ;
#2363 = VECTOR ( 'NONE', #7257, 1000.000000000000000 ) ;
#2364 = ADVANCED_FACE ( 'NONE', ( #13069 ), #312, .F. ) ;
#2365 = PLANE ( 'NONE',  #17326 ) ;
#2366 = CARTESIAN_POINT ( 'NONE',  ( 1.884282074604925583, -8.375506800461993251, 2.375363417140690547 ) ) ;
#2367 = DIRECTION ( 'NONE',  ( 1.000000000000000000, 0.000000000000000000, 0.000000000000000000 ) ) ;
#2368 = AXIS2_PLACEMENT_3D ( 'NONE', #5168, #11450, #13524 ) ;
#2369 = CARTESIAN_POINT ( 'NONE',  ( 12.62499999999998401, -20.99999999999999645, 3.146526952850934755 ) ) ;
#2370 = CARTESIAN_POINT ( 'NONE',  ( -19.48630159782011262, 0.000000000000000000, 0.000000000000000000 ) ) ;
#2371 = CARTESIAN_POINT ( 'NONE',  ( 5.409691417683178294, -21.32581373872474373, 5.270995438708348857 ) ) ;
#2372 = CARTESIAN_POINT ( 'NONE',  ( 0.000000000000000000, 11.64110105645932691, 10.00000000000000000 ) ) ;
#2373 = CARTESIAN_POINT ( 'NONE',  ( -7.847191417683175629, -21.53509896474923835, 2.520995438708346192 ) ) ;
#2374 = CARTESIAN_POINT ( 'NONE',  ( -12.15969141768317918, -22.98484643305507191, 0.9790045612916508100 ) ) ;
#2375 = ORIENTED_EDGE ( 'NONE', *, *, #13312, .F. ) ;
#2376 = CARTESIAN_POINT ( 'NONE',  ( 12.63478567848856571, -19.00582323632600890, 4.762720106674273701 ) ) ;
#2377 = CARTESIAN_POINT ( 'NONE',  ( -13.10821839766814279, 4.152529082241303904, 5.997503362667785609 ) ) ;
#2378 = ORIENTED_EDGE ( 'NONE', *, *, #19426, .F. ) ;
#2379 = VECTOR ( 'NONE', #18013, 1000.000000000000000 ) ;
#2380 = CARTESIAN_POINT ( 'NONE',  ( -20.75349085826862350, 10.00000000000000000, 0.000000000000000000 ) ) ;
#2381 = FACE_OUTER_BOUND ( 'NONE', #2142, .T. ) ;
#2382 = B_SPLINE_CURVE_WITH_KNOTS ( 'NONE', 3,
 ( #3343, #3238, #8058, #9312, #12753, #11095, #3041, #19356, #106, #6492, #10988, #4596, #17780, #1370, #3142, #9722, #15887, #7942, #18941, #7751, #20522, #9419, #6175, #14312, #19156, #4811, #11190, #17565, #9610, #3447, #16599, #5527, #18092, #7000, #14738, #19464, #11800, #16210, #3649, #8669, #3854, #13261, #2278, #8469, #5216, #414, #13063, #723, #19770, #5119, #9825, #1877, #10135, #19657, #6892, #15039, #3757, #11898, #14838, #16507, #17978, #8260, #14625, #10031, #2181, #13367, #5429, #6796, #308, #17879, #18189, #5322, #512, #11694, #10233, #7107, #13164, #19563, #6693, #11499, #8564, #13471 ),
 .UNSPECIFIED., .F., .F.,
 ( 4, 2, 2, 2, 2, 2, 2, 2, 2, 2, 2, 2, 2, 2, 2, 2, 2, 2, 2, 2, 2, 2, 2, 2, 2, 2, 2, 2, 2, 2, 2, 2, 2, 2, 2, 2, 2, 2, 2, 2, 4 ),
 ( 0.03648247254878290990, 0.05122453910963482848, 0.05943139484297973313, 0.06353482270965218892, 0.06763825057632463778, 0.07081696859385248899, 0.07399568661138034020, 0.08035312264643605651, 0.09306799471654747524, 0.1057828667866588801, 0.1121403028217145964, 0.1153190208392424337, 0.1184977388567702850, 0.1214804596100246964, 0.1244631803632790940, 0.1304286218697879030, 0.1423595048828055210, 0.1662212709088407014, 0.2139448029609111179, 0.3093918670650518954, 0.5002859952733336169, 0.6911801234816151718, 0.7866271875857560048, 0.8343507196378263657, 0.8582124856638615462, 0.8701433686768791365, 0.8761088101833880426, 0.8790915309366424957, 0.8820742516898969487, 0.8853411830926060100, 0.8886081144953148492, 0.8951419773007329717, 0.9082097029115692166, 0.9212774285224054616, 0.9278112913278236951, 0.9310782227305326453, 0.9343451541332417065, 0.9384485819999140999, 0.9425520098665866042, 0.9507588655999313909, 0.9671725770666211863 ),
 .UNSPECIFIED. ) ;
#2383 = ORIENTED_EDGE ( 'NONE', *, *, #1435, .T. ) ;
#2384 = ORIENTED_EDGE ( 'NONE', *, *, #12976, .F. ) ;
#2385 = ORIENTED_EDGE ( 'NONE', *, *, #2109, .F. ) ;
#2386 = CARTESIAN_POINT ( 'NONE',  ( 6.813547257480585095, 16.00000000000000000, 1.000000000000000000 ) ) ;
#2387 = LINE ( 'NONE', #7419, #6618 ) ;
#2388 = EDGE_CURVE ( 'NONE', #814, #18396, #10689, .T. ) ;
#2389 = CARTESIAN_POINT ( 'NONE',  ( -2.808565762442263303, -10.28561894962424716, 1.923303392614186924 ) ) ;
#2390 = CARTESIAN_POINT ( 'NONE',  ( 10.49999999999999467, -9.999999999999991118, 2.500000000000000000 ) ) ;
#2391 = DIRECTION ( 'NONE',  ( 0.000000000000000000, 1.000000000000000000, -0.000000000000000000 ) ) ;
#2392 = VECTOR ( 'NONE', #17653, 1000.000000000000000 ) ;
#2393 = CARTESIAN_POINT ( 'NONE',  ( -13.49999999999998401, -19.52007894294123957, 12.00000000000000000 ) ) ;
#2394 = CARTESIAN_POINT ( 'NONE',  ( 13.50000000000001243, -18.49999999999999645, 4.000000000000000000 ) ) ;
#2395 = CARTESIAN_POINT ( 'NONE',  ( 4.840308582316795061, -22.98484643305508612, 6.020995438708344416 ) ) ;
#2396 = CARTESIAN_POINT ( 'NONE',  ( -13.05696142222617695, 1.564051822406025583, 5.955108176248398166 ) ) ;
#2397 = CARTESIAN_POINT ( 'NONE',  ( -7.284691417683176518, -24.52099543870834708, 4.484846433055073689 ) ) ;
#2398 = ORIENTED_EDGE ( 'NONE', *, *, #18015, .F. ) ;
#2399 = CARTESIAN_POINT ( 'NONE',  ( 10.55905858231679595, -20.72672167713054137, 4.701595411283463477 ) ) ;
#2400 = DIRECTION ( 'NONE',  ( 0.000000000000000000, -0.8660254037844363761, 0.5000000000000041078 ) ) ;
#2401 = CARTESIAN_POINT ( 'NONE',  ( -13.40322194933353828, -19.57479155865495457, 6.214283636730510096 ) ) ;
#2402 = EDGE_CURVE ( 'NONE', #19322, #8256, #5179, .T. ) ;
#2403 = CARTESIAN_POINT ( 'NONE',  ( 5.684058582316795949, -21.32873467460644079, 2.757051763020455404 ) ) ;
#2404 = CARTESIAN_POINT ( 'NONE',  ( -1.437849085826860884, 11.64110105645932691, 10.00000000000000000 ) ) ;
#2405 = EDGE_LOOP ( 'NONE', ( #11894, #6714, #11003, #19452 ) ) ;
#2406 = EDGE_LOOP ( 'NONE', ( #4004, #9820, #889, #20540 ) ) ;
#2407 = CARTESIAN_POINT ( 'NONE',  ( 13.40022353639839103, -18.97621141187856608, 5.498856782956575984 ) ) ;
#2408 = FACE_OUTER_BOUND ( 'NONE', #17328, .T. ) ;
#2409 = VERTEX_POINT ( 'NONE', #14939 ) ;
#2410 = AXIS2_PLACEMENT_3D ( 'NONE', #17620, #3290, #1521 ) ;
#2411 = DIRECTION ( 'NONE',  ( -0.000000000000000000, -0.000000000000000000, -1.000000000000000000 ) ) ;
#2412 = PLANE ( 'NONE',  #10370 ) ;
#2413 = PLANE ( 'NONE',  #3971 ) ;
#2414 = CARTESIAN_POINT ( 'NONE',  ( 13.37500015856764435, -20.24999199233421265, 4.532157119432948633 ) ) ;
#2415 = DIRECTION ( 'NONE',  ( 1.000000000000000000, 0.000000000000000000, 0.000000000000000000 ) ) ;
#2416 = CARTESIAN_POINT ( 'NONE',  ( 1.407845757905374695, -8.364917468222230923, 2.372643865078341019 ) ) ;
#2417 = PLANE ( 'NONE',  #1043 ) ;
#2418 = CARTESIAN_POINT ( 'NONE',  ( -12.62506359033936754, -19.49678868786235597, 4.541393094775662220 ) ) ;
#2419 = CARTESIAN_POINT ( 'NONE',  ( 0.000000000000000000, 4.999999999999999112, 1.000000000000000000 ) ) ;
#2420 = CARTESIAN_POINT ( 'NONE',  ( 11.40280858231679417, -22.77556120703056308, 1.770995438708339975 ) ) ;
#2421 = CARTESIAN_POINT ( 'NONE',  ( -13.38172782443493602, -20.66024486603417643, 5.557997437521964734 ) ) ;
#2422 = VECTOR ( 'NONE', #3088, 1000.000000000000000 ) ;
#2423 = DIRECTION ( 'NONE',  ( -1.000000000000000000, 0.000000000000000000, 0.000000000000000000 ) ) ;
#2424 = CARTESIAN_POINT ( 'NONE',  ( 4.717959273841179524, -21.82295283170803302, 4.493595146365858994 ) ) ;
#2425 = CARTESIAN_POINT ( 'NONE',  ( 11.03469141768317741, -20.97900456129164581, 3.136473910504570917 ) ) ;
#2426 = CARTESIAN_POINT ( 'NONE',  ( -13.37155858231679417, -20.24999999999999289, 3.449312527122348371 ) ) ;
#2427 = ORIENTED_EDGE ( 'NONE', *, *, #19253, .T. ) ;
#2428 = CARTESIAN_POINT ( 'NONE',  ( 12.73577686058281344, -15.40576854059989920, 6.340204579155907183 ) ) ;
#2429 = CARTESIAN_POINT ( 'NONE',  ( 12.62500000000002132, -19.49999999999450040, 3.833333333368183382 ) ) ;
#2430 = CARTESIAN_POINT ( 'NONE',  ( 20.49999999999998224, -21.99999999999999645, 9.999999999999998224 ) ) ;
#2431 = ORIENTED_EDGE ( 'NONE', *, *, #4015, .T. ) ;
#2432 = EDGE_CURVE ( 'NONE', #14519, #13440, #3550, .T. ) ;
#2433 = EDGE_LOOP ( 'NONE', ( #819, #7865, #10309, #10304 ) ) ;
#2434 = DIRECTION ( 'NONE',  ( 1.000000000000000000, 0.000000000000000000, -0.000000000000000000 ) ) ;
#2435 = AXIS2_PLACEMENT_3D ( 'NONE', #12950, #14735, #19767 ) ;
#2436 = CARTESIAN_POINT ( 'NONE',  ( 6.063547257480584207, 0.000000000000000000, 0.000000000000000000 ) ) ;
#2437 = LINE ( 'NONE', #15195, #968 ) ;
#2438 = LINE ( 'NONE', #18867, #372 ) ;
#2439 = CARTESIAN_POINT ( 'NONE',  ( 1.957016269584227031, -9.152392576945766578, 2.382268221639079364 ) ) ;
#2440 = DIRECTION ( 'NONE',  ( 1.000000000000000000, 0.000000000000000000, -0.000000000000000000 ) ) ;
#2441 = CARTESIAN_POINT ( 'NONE',  ( -1.561130159782011306, 9.000000000000001776, 0.000000000000000000 ) ) ;
#2442 = CARTESIAN_POINT ( 'NONE',  ( -14.56494360078803396, 16.00000000000000000, 1.000000000000000000 ) ) ;
#2443 = CARTESIAN_POINT ( 'NONE',  ( -7.652808582316795061, -21.22443879296942626, 5.229004561291659137 ) ) ;
#2444 = CARTESIAN_POINT ( 'NONE',  ( -1.513434189748285918, -8.364917468222230923, 1.622643865078341907 ) ) ;
#2445 = VERTEX_POINT ( 'NONE', #10238 ) ;
#2446 = CARTESIAN_POINT ( 'NONE',  ( -13.37499999999998401, -19.49999999999998934, 3.666666666666654084 ) ) ;
#2447 = CARTESIAN_POINT ( 'NONE',  ( -5.402808582316794173, -22.77556120703056308, 1.770995438708339975 ) ) ;
#2448 = CARTESIAN_POINT ( 'NONE',  ( 8.402808582316797725, -23.08622137881038938, 1.020995438708339309 ) ) ;
#2449 = CARTESIAN_POINT ( 'NONE',  ( -10.28469141768317741, -23.02099543870834353, 3.863526089495429972 ) ) ;
#2450 = ORIENTED_EDGE ( 'NONE', *, *, #15273, .T. ) ;
#2451 = CARTESIAN_POINT ( 'NONE',  ( 13.85788212999909419, 4.135547564954428879, 5.982801014393342776 ) ) ;
#2452 = LINE ( 'NONE', #789, #14727 ) ;
#2453 = VERTEX_POINT ( 'NONE', #1780 ) ;
#2454 = ORIENTED_EDGE ( 'NONE', *, *, #4226, .T. ) ;
#2455 = CARTESIAN_POINT ( 'NONE',  ( 15.50000000000002132, -26.49999999999999645, 1.000000000000000000 ) ) ;
#2456 = ADVANCED_FACE ( 'NONE', ( #19567 ), #8167, .T. ) ;
#2457 = ORIENTED_EDGE ( 'NONE', *, *, #4151, .T. ) ;
#2458 = CARTESIAN_POINT ( 'NONE',  ( 12.00000000000000178, -26.50000000000000355, 1.000000000000000000 ) ) ;
#2459 = ADVANCED_FACE ( 'NONE', ( #11598 ), #17983, .T. ) ;
#2460 = EDGE_CURVE ( 'NONE', #7326, #20051, #16369, .T. ) ;
#2461 = VERTEX_POINT ( 'NONE', #8263 ) ;
#2462 = PLANE ( 'NONE',  #5271 ) ;
#2463 = DIRECTION ( 'NONE',  ( 1.000000000000000000, -0.000000000000000000, 0.000000000000000000 ) ) ;
#2464 = LINE ( 'NONE', #4042, #297 ) ;
#2465 = CARTESIAN_POINT ( 'NONE',  ( 3.636036383999129207, -10.90885478516162976, 2.275977788322152584 ) ) ;
#2466 = CARTESIAN_POINT ( 'NONE',  ( 0.000000000000000000, 11.64110105645932691, 0.000000000000000000 ) ) ;
#2467 = EDGE_CURVE ( 'NONE', #19883, #3190, #5533, .T. ) ;
#2468 = CARTESIAN_POINT ( 'NONE',  ( 13.90434039801927568, 5.731690099970989216, 5.115558489342345361 ) ) ;
#2469 = CARTESIAN_POINT ( 'NONE',  ( 5.000000000000000000, -12.50000000000000000, 1.000000000000000000 ) ) ;
#2470 = CARTESIAN_POINT ( 'NONE',  ( 11.03469141768317741, -20.97900456129164581, 3.136473910504570917 ) ) ;
#2471 = DIRECTION ( 'NONE',  ( 1.000000000000000000, -0.000000000000000000, 0.000000000000000000 ) ) ;
#2472 = CARTESIAN_POINT ( 'NONE',  ( -7.753441417683177406, -21.94931252712233061, 2.499999999999999112 ) ) ;
#2473 = CARTESIAN_POINT ( 'NONE',  ( -8.597191417683177406, -23.08622137881040359, 5.979004561291654696 ) ) ;
#2474 = ORIENTED_EDGE ( 'NONE', *, *, #4002, .T. ) ;
#2475 = CARTESIAN_POINT ( 'NONE',  ( 13.12529397354238192, 5.014845663890295846, 4.666666666666619889 ) ) ;
#2476 = CARTESIAN_POINT ( 'NONE',  ( -12.74043380832193684, -14.42059267975384529, 5.611358176248560703 ) ) ;
#2477 = VERTEX_POINT ( 'NONE', #18608 ) ;
#2478 = FACE_OUTER_BOUND ( 'NONE', #13298, .T. ) ;
#2479 = EDGE_CURVE ( 'NONE', #17198, #4223, #8882, .T. ) ;
#2480 = DIRECTION ( 'NONE',  ( 1.000000000000000000, 0.000000000000000000, 0.000000000000000000 ) ) ;
#2481 = VERTEX_POINT ( 'NONE', #12318 ) ;
#2482 = VERTEX_POINT ( 'NONE', #7113 ) ;
#2483 = VERTEX_POINT ( 'NONE', #12219 ) ;
#2484 = DIRECTION ( 'NONE',  ( 0.000000000000000000, 1.000000000000000000, 0.000000000000000000 ) ) ;
#2485 = DIRECTION ( 'NONE',  ( 1.000000000000000000, 0.000000000000000000, 0.000000000000000000 ) ) ;
#2486 = CARTESIAN_POINT ( 'NONE',  ( -2.747777887823422471, -9.906471667804277459, 1.825930796414880763 ) ) ;
#2487 = DIRECTION ( 'NONE',  ( -0.000000000000000000, 0.000000000000000000, -1.000000000000000000 ) ) ;
#2488 = CARTESIAN_POINT ( 'NONE',  ( 10.05565079891005631, 9.000000000000001776, 1.000000000000000000 ) ) ;
#2489 = DIRECTION ( 'NONE',  ( -1.000000000000000000, 0.000000000000000000, 0.000000000000000000 ) ) ;
#2490 = CARTESIAN_POINT ( 'NONE',  ( 5.215308582316795949, -24.52099543870834708, 2.515153566944913432 ) ) ;
#2491 = CARTESIAN_POINT ( 'NONE',  ( -13.08573665985359824, 3.017201322601628100, 5.986358176248492313 ) ) ;
#2492 = CARTESIAN_POINT ( 'NONE',  ( -4.284691417683177406, -24.52099543870834708, 4.484846433055073689 ) ) ;
#2493 = EDGE_LOOP ( 'NONE', ( #630, #1999, #10925, #15522 ) ) ;
#2494 = PLANE ( 'NONE',  #20651 ) ;
#2495 = CARTESIAN_POINT ( 'NONE',  ( 11.00000000000000000, -24.49999999999999289, 5.000000000000000000 ) ) ;
#2496 = CARTESIAN_POINT ( 'NONE',  ( -13.89730118381875279, 5.376209782841177898, 6.083536567043803522 ) ) ;
#2497 = CARTESIAN_POINT ( 'NONE',  ( 5.871558582316795949, -20.99999999999999645, 3.449312527122348371 ) ) ;
#2498 = EDGE_CURVE ( 'NONE', #9688, #610, #8982, .T. ) ;
#2499 = DIRECTION ( 'NONE',  ( 0.000000000000000000, 0.000000000000000000, 1.000000000000000000 ) ) ;
#2500 = VERTEX_POINT ( 'NONE', #17028 ) ;
#2501 = EDGE_CURVE ( 'NONE', #6659, #14414, #4070, .T. ) ;
#2502 = ORIENTED_EDGE ( 'NONE', *, *, #338, .T. ) ;
#2503 = CARTESIAN_POINT ( 'NONE',  ( 13.87467358130843387, 4.983515856073828409, 5.065827972856573602 ) ) ;
#2504 = VECTOR ( 'NONE', #11042, 1000.000000000000000 ) ;
#2505 = CARTESIAN_POINT ( 'NONE',  ( -0.000000000000000000, 11.64110105645932691, 0.000000000000000000 ) ) ;
#2506 =( NAMED_UNIT ( * ) SI_UNIT ( $, .STERADIAN. ) SOLID_ANGLE_UNIT ( ) );
#2507 = ORIENTED_EDGE ( 'NONE', *, *, #19909, .F. ) ;
#2508 = CARTESIAN_POINT ( 'NONE',  ( -3.999999999999999112, -2.500000000000047518, 7.000000000000000000 ) ) ;
#2509 = PLANE ( 'NONE',  #2345 ) ;
#2510 = CARTESIAN_POINT ( 'NONE',  ( -14.49999999999998579, -24.49999999999999289, 1.000000000000000000 ) ) ;
#2511 = CARTESIAN_POINT ( 'NONE',  ( 13.86470821076586368, 4.480264643675554659, 5.874551681240599343 ) ) ;
#2512 = VECTOR ( 'NONE', #15224, 1000.000000000000000 ) ;
#2513 = CARTESIAN_POINT ( 'NONE',  ( 25.54469207716615031, 9.000000000000001776, 0.000000000000000000 ) ) ;
#2514 = CARTESIAN_POINT ( 'NONE',  ( 3.347120161770001268, -14.10934257735911146, 2.905312006771028077 ) ) ;
#2515 = ADVANCED_FACE ( 'NONE', ( #16604 ), #7212, .T. ) ;
#2516 = DIRECTION ( 'NONE',  ( -1.156482317317871331E-15, 1.000000000000000000, -0.000000000000000000 ) ) ;
#2517 = CARTESIAN_POINT ( 'NONE',  ( -12.62499999999998401, -19.49999999999998934, 3.666666666666654084 ) ) ;
#2518 = CARTESIAN_POINT ( 'NONE',  ( 0.000000000000000000, 9.000000000000001776, 1.000000000000000000 ) ) ;
#2519 = CARTESIAN_POINT ( 'NONE',  ( -13.41355111217617413, -19.05316883510194614, 6.247234435864091218 ) ) ;
#2520 = PLANE ( 'NONE',  #15720 ) ;
#2521 = CARTESIAN_POINT ( 'NONE',  ( 12.05905858231679417, -20.72672167713054137, 4.701595411283463477 ) ) ;
#2522 = CARTESIAN_POINT ( 'NONE',  ( 4.097191417683176518, -22.77556120703057729, 5.229004561291655584 ) ) ;
#2523 = CARTESIAN_POINT ( 'NONE',  ( -10.55905858231679595, -20.72672167713054137, 4.701595411283463477 ) ) ;
#2524 = ORIENTED_EDGE ( 'NONE', *, *, #13066, .T. ) ;
#2525 = CARTESIAN_POINT ( 'NONE',  ( 13.04271272860988340, 0.09449279482665236263, 6.673537912489449830 ) ) ;
#2526 = CARTESIAN_POINT ( 'NONE',  ( 13.09001666039658573, 3.983341349998239966, 5.257104358157307367 ) ) ;
#2527 = CYLINDRICAL_SURFACE ( 'NONE', #12346, 10.00000000000000000 ) ;
#2528 = ORIENTED_EDGE ( 'NONE', *, *, #3640, .F. ) ;
#2529 = UNCERTAINTY_MEASURE_WITH_UNIT (LENGTH_MEASURE( 1.000000000000000082E-05 ), #17942, 'distance_accuracy_value', 'NONE');
#2530 = ORIENTED_EDGE ( 'NONE', *, *, #20355, .F. ) ;
#2531 = CARTESIAN_POINT ( 'NONE',  ( 0.000000000000000000, 4.999999999999999112, 1.000000000000000000 ) ) ;
#2532 = CIRCLE ( 'NONE', #10562, 10.00000000000000000 ) ;
#2533 = CARTESIAN_POINT ( 'NONE',  ( -12.74043380832193684, -14.42059267975384529, 5.611358176248560703 ) ) ;
#2534 = DIRECTION ( 'NONE',  ( -0.000000000000000000, -0.000000000000000000, -1.000000000000000000 ) ) ;
#2535 = CARTESIAN_POINT ( 'NONE',  ( -13.41341218697771609, -18.31018455762212227, 5.513179699623425023 ) ) ;
#2536 = EDGE_CURVE ( 'NONE', #15304, #15313, #10456, .T. ) ;
#2537 = DIRECTION ( 'NONE',  ( 0.000000000000000000, 1.000000000000000000, -0.000000000000000000 ) ) ;
#2538 = CARTESIAN_POINT ( 'NONE',  ( 2.579281110863027582, -9.822567596814183233, 2.554382554832406615 ) ) ;
#2539 = CARTESIAN_POINT ( 'NONE',  ( 13.00209451496117374, 16.00000000000000000, 1.000000000000000000 ) ) ;
#2540 = CARTESIAN_POINT ( 'NONE',  ( 17.11324865405191176, -10.99999999999999645, 1.000000000000000000 ) ) ;
#2541 =( BOUNDED_CURVE ( )  B_SPLINE_CURVE ( 3, ( #18318, #3674, #14860, #5346 ),
 .UNSPECIFIED., .F., .F. ) 
 B_SPLINE_CURVE_WITH_KNOTS ( ( 4, 4 ),
 ( 1.468430546537837468E-05, 0.001172421487176120289 ),
 .UNSPECIFIED. ) 
 CURVE ( )  GEOMETRIC_REPRESENTATION_ITEM ( )  RATIONAL_B_SPLINE_CURVE ( ( 0.9619191252709937690, 0.3335846922424353656, 0.3462783171521043313, 1.000000000000000222 ) ) 
 REPRESENTATION_ITEM ( '' )  );
#2542 = CARTESIAN_POINT ( 'NONE',  ( -1.337453470010121714, -9.114917468222230923, 2.372643865078341019 ) ) ;
#2543 = CARTESIAN_POINT ( 'NONE',  ( -9.434058582316795949, -23.73192549717337130, 5.303608408759367343 ) ) ;
#2544 = CARTESIAN_POINT ( 'NONE',  ( -2.708677329869237482, -9.785633270066144362, 1.794897081886200230 ) ) ;
#2545 = ORIENTED_EDGE ( 'NONE', *, *, #4304, .F. ) ;
#2546 = VECTOR ( 'NONE', #1113, 1000.000000000000000 ) ;
#2547 = CARTESIAN_POINT ( 'NONE',  ( -13.37593719518949698, -19.45267164293252193, 4.647380496992003174 ) ) ;
#2548 = DIRECTION ( 'NONE',  ( -1.000000000000000000, -1.156482317317871133E-15, 0.000000000000000000 ) ) ;
#2549 = CARTESIAN_POINT ( 'NONE',  ( 12.53469141768317741, -19.47900456129164581, 2.515153566944927199 ) ) ;
#2550 = CARTESIAN_POINT ( 'NONE',  ( -10.37844141768317741, -22.99999999999999645, 3.449312527122335048 ) ) ;
#2551 = ORIENTED_EDGE ( 'NONE', *, *, #13882, .F. ) ;
#2552 = EDGE_CURVE ( 'NONE', #12182, #7127, #19879, .T. ) ;
#2553 = CARTESIAN_POINT ( 'NONE',  ( 13.37499999998404121, -20.24999999996810729, 2.793053905886972998 ) ) ;
#2554 = LINE ( 'NONE', #11866, #9386 ) ;
#2555 = ORIENTED_EDGE ( 'NONE', *, *, #1486, .T. ) ;
#2556 = ORIENTED_EDGE ( 'NONE', *, *, #1394, .T. ) ;
#2557 = DIRECTION ( 'NONE',  ( 0.000000000000000000, 1.000000000000000000, -0.000000000000000000 ) ) ;
#2558 = ORIENTED_EDGE ( 'NONE', *, *, #15684, .F. ) ;
#2559 = CARTESIAN_POINT ( 'NONE',  ( -13.86470821076586368, 4.480264643675554659, 5.874551681240599343 ) ) ;
#2560 = CIRCLE ( 'NONE', #4240, 10.00000000000000000 ) ;
#2561 = ORIENTED_EDGE ( 'NONE', *, *, #16454, .F. ) ;
#2562 = DIRECTION ( 'NONE',  ( 0.000000000000000000, -1.000000000000000000, 0.000000000000000000 ) ) ;
#2563 = DIRECTION ( 'NONE',  ( 1.000000000000000000, 8.673617379884033500E-16, -0.000000000000000000 ) ) ;
#2564 = CARTESIAN_POINT ( 'NONE',  ( 11.49178095869207006, 4.999999999999999112, 1.000000000000000000 ) ) ;
#2565 = CARTESIAN_POINT ( 'NONE',  ( 0.5631383031621635116, -8.364917468222230923, 2.372643865078341019 ) ) ;
#2566 = DIRECTION ( 'NONE',  ( 0.000000000000000000, 0.000000000000000000, 1.000000000000000000 ) ) ;
#2567 = ADVANCED_FACE ( 'NONE', ( #7522 ), #18406, .T. ) ;
#2568 = CARTESIAN_POINT ( 'NONE',  ( 13.89992416064626646, 5.508670112635706495, 5.888743936161951353 ) ) ;
#2569 = CARTESIAN_POINT ( 'NONE',  ( -14.49999999999998579, -19.49999999999999645, 4.000000000000000000 ) ) ;
#2570 = DIRECTION ( 'NONE',  ( -1.000000000000000000, -1.156482317317871725E-16, -0.000000000000000000 ) ) ;
#2571 = CARTESIAN_POINT ( 'NONE',  ( 13.12529397354238192, 5.014845663890295846, 4.833333333333344584 ) ) ;
#2572 = CARTESIAN_POINT ( 'NONE',  ( 9.440941417683177406, -21.25705176302044208, 2.828734674606458555 ) ) ;
#2573 = LINE ( 'NONE', #12099, #8892 ) ;
#2574 = CARTESIAN_POINT ( 'NONE',  ( -7.659691417683177406, -22.36352608949543352, 2.479004561291652031 ) ) ;
#2575 = CARTESIAN_POINT ( 'NONE',  ( -4.746558582316795061, -21.94931252712234127, 6.000000000000001776 ) ) ;
#2576 = VERTEX_POINT ( 'NONE', #15251 ) ;
#2577 = EDGE_CURVE ( 'NONE', #12897, #13753, #925, .T. ) ;
#2578 = CARTESIAN_POINT ( 'NONE',  ( 12.62525331949183105, -19.48720736566255951, 4.581880915780448760 ) ) ;
#2579 = CARTESIAN_POINT ( 'NONE',  ( -12.64571531779736979, -19.20387645123237164, 5.508493592915143289 ) ) ;
#2580 = VERTEX_POINT ( 'NONE', #19976 ) ;
#2582 = ADVANCED_FACE ( 'NONE', ( #5637 ), #18295, .T. ) ;
#2581 = AXIS2_PLACEMENT_3D ( 'NONE', #1064, #13594, #13906 ) ;
#2583 = CARTESIAN_POINT ( 'NONE',  ( 25.54469207716615031, 9.000000000000001776, 1.000000000000000000 ) ) ;
#2584 = LINE ( 'NONE', #9660, #5003 ) ;
#2585 = ORIENTED_EDGE ( 'NONE', *, *, #14183, .T. ) ;
#2586 = CARTESIAN_POINT ( 'NONE',  ( 2.534747216115884161, -9.671180236796224960, 2.515503256513427210 ) ) ;
#2587 = ORIENTED_EDGE ( 'NONE', *, *, #10224, .T. ) ;
#2588 = ORIENTED_EDGE ( 'NONE', *, *, #1207, .T. ) ;
#2589 = CARTESIAN_POINT ( 'NONE',  ( 0.000000000000000000, 4.999999999999999112, 1.000000000000000000 ) ) ;
#2590 = CARTESIAN_POINT ( 'NONE',  ( -1.561130159782011306, 4.999999999999999112, 0.000000000000000000 ) ) ;
#2591 = CARTESIAN_POINT ( 'NONE',  ( -1.859341899742023463, -9.902476528685241419, 1.632289782122827271 ) ) ;
#2592 = CARTESIAN_POINT ( 'NONE',  ( 8.876396343307449754, 10.00000000000000000, 1.000000000000000000 ) ) ;
#2593 = FACE_OUTER_BOUND ( 'NONE', #3647, .T. ) ;
#2594 = VECTOR ( 'NONE', #4166, 1000.000000000000000 ) ;
#2595 = EDGE_CURVE ( 'NONE', #7178, #9560, #20082, .T. ) ;
#2596 = DIRECTION ( 'NONE',  ( -1.000000000000000000, 0.000000000000000000, 0.000000000000000000 ) ) ;
#2597 = CARTESIAN_POINT ( 'NONE',  ( 5.402808582316795949, -23.08622137881038938, 1.020995438708339309 ) ) ;
#2598 = CARTESIAN_POINT ( 'NONE',  ( -12.79798428357658047, -11.51429367935891790, 5.673858176248284479 ) ) ;
#2599 = CARTESIAN_POINT ( 'NONE',  ( -5.222191417683177406, -19.52099543870834353, 4.586221378810406257 ) ) ;
#2600 = ORIENTED_EDGE ( 'NONE', *, *, #7451, .T. ) ;
#2601 = CARTESIAN_POINT ( 'NONE',  ( 11.40280858231679417, -22.77556120703056308, 1.770995438708339975 ) ) ;
#2602 = DIRECTION ( 'NONE',  ( 0.000000000000000000, 0.8660254037844363761, -0.5000000000000041078 ) ) ;
#2603 = CARTESIAN_POINT ( 'NONE',  ( -13.41115317570721110, -19.17426462678482579, 6.244630269197427808 ) ) ;
#2604 = CARTESIAN_POINT ( 'NONE',  ( 5.590308582316795949, -21.63647391050454871, 2.479004561291657804 ) ) ;
#2605 = CARTESIAN_POINT ( 'NONE',  ( 4.247260319564023945, 0.000000000000000000, 0.000000000000000000 ) ) ;
#2606 = ORIENTED_EDGE ( 'NONE', *, *, #11830, .T. ) ;
#2607 = VERTEX_POINT ( 'NONE', #15044 ) ;
#2608 = CARTESIAN_POINT ( 'NONE',  ( 13.50467269799730374, -14.45152875114793467, 6.346192769197517514 ) ) ;
#2609 = CARTESIAN_POINT ( 'NONE',  ( -5.563547257480587760, 0.000000000000000000, 0.000000000000000000 ) ) ;
#2610 = CARTESIAN_POINT ( 'NONE',  ( 0.000000000000000000, 0.000000000000000000, 0.000000000000000000 ) ) ;
#2611 = EDGE_LOOP ( 'NONE', ( #2600, #7746, #1044, #15474 ) ) ;
#2612 = VECTOR ( 'NONE', #15562, 1000.000000000000000 ) ;
#2613 = DIRECTION ( 'NONE',  ( 0.000000000000000000, 0.000000000000000000, -1.000000000000000000 ) ) ;
#2614 = ORIENTED_EDGE ( 'NONE', *, *, #1886, .T. ) ;
#2615 = CARTESIAN_POINT ( 'NONE',  ( -12.62155858231679417, -23.74999999999999645, 3.550687472877651629 ) ) ;
#2616 = CARTESIAN_POINT ( 'NONE',  ( 22.56633994409548194, 10.00000000000000000, 0.000000000000000000 ) ) ;
#2617 = LINE ( 'NONE', #15380, #14540 ) ;
#2618 = CARTESIAN_POINT ( 'NONE',  ( 2.739050625766161762, -9.875938058683834342, 1.818089155622620412 ) ) ;
#2619 = EDGE_CURVE ( 'NONE', #13746, #4108, #3958, .T. ) ;
#2620 = EDGE_CURVE ( 'NONE', #15262, #2170, #13674, .T. ) ;
#2621 = DIRECTION ( 'NONE',  ( 0.000000000000000000, -1.000000000000000000, 0.000000000000000000 ) ) ;
#2622 = CARTESIAN_POINT ( 'NONE',  ( -13.37505992445764136, -19.49697381488866554, 4.539006848837218833 ) ) ;
#2623 = AXIS2_PLACEMENT_3D ( 'NONE', #3905, #10283, #16654 ) ;
#2624 = VECTOR ( 'NONE', #19131, 1000.000000000000000 ) ;
#2625 = LINE ( 'NONE', #4410, #19437 ) ;
#2626 = CARTESIAN_POINT ( 'NONE',  ( -13.37505392270939986, -20.99727690317663686, 4.612442573673130930 ) ) ;
#2627 = CIRCLE ( 'NONE', #16989, 0.2500000000000002220 ) ;
#2628 = EDGE_CURVE ( 'NONE', #9247, #9180, #10346, .T. ) ;
#2629 = DIRECTION ( 'NONE',  ( -0.000000000000000000, 0.000000000000000000, -1.000000000000000000 ) ) ;
#2630 = CARTESIAN_POINT ( 'NONE',  ( 10.27780858231679417, -20.27099543870833642, 2.724438792969431589 ) ) ;
#2631 = AXIS2_PLACEMENT_3D ( 'NONE', #12717, #13973, #6041 ) ;
#2632 = CARTESIAN_POINT ( 'NONE',  ( 11.50344141768317741, -22.05068747287766229, 4.499999999999999112 ) ) ;
#2633 = CARTESIAN_POINT ( 'NONE',  ( -8.684058582316794173, -20.79840458871652942, 2.226721677130544030 ) ) ;
#2634 = ORIENTED_EDGE ( 'NONE', *, *, #2145, .F. ) ;
#2635 = CARTESIAN_POINT ( 'NONE',  ( 13.37499999999998401, -19.49999999999998934, 3.146526952850934755 ) ) ;
#2636 = FACE_OUTER_BOUND ( 'NONE', #1256, .T. ) ;
#2637 = ORIENTED_EDGE ( 'NONE', *, *, #1172, .T. ) ;
#2638 = EDGE_CURVE ( 'NONE', #2482, #2481, #16717, .T. ) ;
#2639 = VERTEX_POINT ( 'NONE', #16922 ) ;
#2640 = LINE ( 'NONE', #20127, #14451 ) ;
#2641 = VECTOR ( 'NONE', #4244, 1000.000000000000114 ) ;
#2642 = CARTESIAN_POINT ( 'NONE',  ( -13.08094078691552831, 2.775009739235173356, 5.981149842915306714 ) ) ;
#2643 = VECTOR ( 'NONE', #7124, 1000.000000000000000 ) ;
#2644 = CARTESIAN_POINT ( 'NONE',  ( -2.616536356806028696, -10.07836329504444706, 2.620076000170431296 ) ) ;
#2645 = CARTESIAN_POINT ( 'NONE',  ( -13.39482594849551944, -19.24878960097397140, 5.493002502378098839 ) ) ;
#2646 = DIRECTION ( 'NONE',  ( 0.000000000000000000, 0.000000000000000000, 1.000000000000000000 ) ) ;
#2647 = CARTESIAN_POINT ( 'NONE',  ( 0.000000000000000000, 4.999999999999999112, 1.000000000000000000 ) ) ;
#2648 = CARTESIAN_POINT ( 'NONE',  ( 2.499999999999998668, -19.49999999999999645, 4.000000000000000000 ) ) ;
#2649 = CARTESIAN_POINT ( 'NONE',  ( -9.000000000000000000, -9.999999999999992895, 2.000000000000000000 ) ) ;
#2650 = CARTESIAN_POINT ( 'NONE',  ( -18.69064177244175795, 0.000000000000000000, 0.000000000000000000 ) ) ;
#2651 = CARTESIAN_POINT ( 'NONE',  ( -4.746558582316793284, -21.94931252712234482, 5.250000000000000888 ) ) ;
#2652 = CIRCLE ( 'NONE', #18354, 10.00000000000000000 ) ;
#2653 = CARTESIAN_POINT ( 'NONE',  ( -3.059891148793807414, -12.07002330923453570, 2.381574079220715401 ) ) ;
#2654 = VERTEX_POINT ( 'NONE', #5850 ) ;
#2655 = CARTESIAN_POINT ( 'NONE',  ( -13.84501469867711698, 4.235742283194553259, 4.833333333333343695 ) ) ;
#2656 = DIRECTION ( 'NONE',  ( 0.000000000000000000, -1.000000000000000000, 0.000000000000000000 ) ) ;
#2657 = CARTESIAN_POINT ( 'NONE',  ( 6.809058582316796837, -23.80360840875935935, 1.768074502826626260 ) ) ;
#2658 = CARTESIAN_POINT ( 'NONE',  ( -10.09719141768317741, -22.46490103525075810, 4.479004561291653808 ) ) ;
#2659 = AXIS2_PLACEMENT_3D ( 'NONE', #4850, #3280, #11333 ) ;
#2660 = ORIENTED_EDGE ( 'NONE', *, *, #3263, .F. ) ;
#2661 = CARTESIAN_POINT ( 'NONE',  ( 13.37499999999998401, -20.24999999999998934, 2.439580858552613751 ) ) ;
#2662 = CYLINDRICAL_SURFACE ( 'NONE', #12380, 0.3750000000000003331 ) ;
#2663 = VERTEX_POINT ( 'NONE', #1144 ) ;
#2664 = EDGE_LOOP ( 'NONE', ( #6791, #7977 ) ) ;
#2665 = EDGE_CURVE ( 'NONE', #3979, #932, #13886, .T. ) ;
#2666 = CARTESIAN_POINT ( 'NONE',  ( -5.433390479346035029, 4.999999999999999112, 0.000000000000000000 ) ) ;
#2667 = AXIS2_PLACEMENT_3D ( 'NONE', #13167, #16514, #14841 ) ;
#2668 = ORIENTED_EDGE ( 'NONE', *, *, #17168, .T. ) ;
#2669 = CARTESIAN_POINT ( 'NONE',  ( -13.81626551376501588, 2.033908445126689557, 5.950679699622869911 ) ) ;
#2670 = CARTESIAN_POINT ( 'NONE',  ( -14.00000000000000000, 0.000000000000000000, 0.5000000000000000000 ) ) ;
#2671 = VECTOR ( 'NONE', #17590, 1000.000000000000000 ) ;
#2672 = ORIENTED_EDGE ( 'NONE', *, *, #20182, .T. ) ;
#2673 = DIRECTION ( 'NONE',  ( 0.000000000000000000, 0.000000000000000000, -1.000000000000000000 ) ) ;
#2674 = CARTESIAN_POINT ( 'NONE',  ( -30.00000000000000000, 0.000000000000000000, 0.000000000000000000 ) ) ;
#2675 =( BOUNDED_CURVE ( )  B_SPLINE_CURVE ( 3, ( #14300, #12944, #1556, #11588 ),
 .UNSPECIFIED., .F., .F. ) 
 B_SPLINE_CURVE_WITH_KNOTS ( ( 4, 4 ),
 ( 0.000000000000000000, 1.468430546537837468E-05 ),
 .UNSPECIFIED. ) 
 CURVE ( )  GEOMETRIC_REPRESENTATION_ITEM ( )  RATIONAL_B_SPLINE_CURVE ( ( 1.000000000000000000, 0.9870550161812301493, 0.9743613912715626268, 0.9619191252709974327 ) ) 
 REPRESENTATION_ITEM ( '' )  );
#2676 = LINE ( 'NONE', #7395, #17000 ) ;
#2677 = CARTESIAN_POINT ( 'NONE',  ( 2.787023586469211001, -10.13267000451481614, 1.884023048047904103 ) ) ;
#2678 = FACE_OUTER_BOUND ( 'NONE', #15058, .T. ) ;
#2679 = AXIS2_PLACEMENT_3D ( 'NONE', #18016, #10170, #16540 ) ;
#2680 = VECTOR ( 'NONE', #5272, 1000.000000000000000 ) ;
#2681 = LINE ( 'NONE', #15538, #11625 ) ;
#2682 = DIRECTION ( 'NONE',  ( 0.000000000000000000, 1.000000000000000000, 0.000000000000000000 ) ) ;
#2683 = CARTESIAN_POINT ( 'NONE',  ( 13.12529397354238192, 5.014845663890295846, 4.333333333333382775 ) ) ;
#2684 = CARTESIAN_POINT ( 'NONE',  ( 12.06594141768317741, -22.67126532539353789, 2.757051763020445634 ) ) ;
#2685 = CARTESIAN_POINT ( 'NONE',  ( -12.63465172146706728, -19.76258806590802664, 5.372658420469845986 ) ) ;
#2686 = CARTESIAN_POINT ( 'NONE',  ( -11.59030858231679595, -21.63647391050454871, 2.479004561291657804 ) ) ;
#2687 = CARTESIAN_POINT ( 'NONE',  ( -4.934058582316795061, -23.73192549717337130, 5.303608408759367343 ) ) ;
#2688 = EDGE_LOOP ( 'NONE', ( #1022, #19401, #17815, #17406 ) ) ;
#2689 = CARTESIAN_POINT ( 'NONE',  ( 13.12529397353891270, 5.014845663890295846, 3.333333333333220239 ) ) ;
#2690 = CARTESIAN_POINT ( 'NONE',  ( -13.12529397354238192, 5.014845663890295846, 3.000000000000000000 ) ) ;
#2691 = VECTOR ( 'NONE', #17232, 1000.000000000000000 ) ;
#2692 = EDGE_LOOP ( 'NONE', ( #16128, #8297 ) ) ;
#2693 = DIRECTION ( 'NONE',  ( -0.000000000000000000, -0.000000000000000000, -1.000000000000000000 ) ) ;
#2694 = CARTESIAN_POINT ( 'NONE',  ( 2.499999999999998668, -19.50000000000000000, 1.000000000000000000 ) ) ;
#2695 = ORIENTED_EDGE ( 'NONE', *, *, #4274, .F. ) ;
#2696 = CARTESIAN_POINT ( 'NONE',  ( 2.731427961995660958, -10.89409100229510052, 2.829571171190552015 ) ) ;
#2697 = VECTOR ( 'NONE', #19430, 1000.000000000000000 ) ;
#2698 = AXIS2_PLACEMENT_3D ( 'NONE', #17310, #1010, #15745 ) ;
#2699 = EDGE_CURVE ( 'NONE', #8463, #13542, #4343, .T. ) ;
#2700 = VERTEX_POINT ( 'NONE', #9880 ) ;
#2701 = DIRECTION ( 'NONE',  ( 0.000000000000000000, -1.000000000000000000, 0.000000000000000000 ) ) ;
#2702 = DIRECTION ( 'NONE',  ( -0.000000000000000000, -0.000000000000000000, -1.000000000000000000 ) ) ;
#2703 = EDGE_CURVE ( 'NONE', #14026, #15081, #10766, .T. ) ;
#2704 = CARTESIAN_POINT ( 'NONE',  ( -2.442511739767545098, -14.09457879449248807, 3.458905389639174821 ) ) ;
#2705 = CARTESIAN_POINT ( 'NONE',  ( 6.813547257480585095, 0.000000000000000000, 0.000000000000000000 ) ) ;
#2706 = DIRECTION ( 'NONE',  ( 0.000000000000000000, 0.000000000000000000, -1.000000000000000000 ) ) ;
#2707 = EDGE_CURVE ( 'NONE', #7093, #14252, #18711, .T. ) ;
#2708 = CARTESIAN_POINT ( 'NONE',  ( -13.81494360078803396, 0.000000000000000000, 1.000000000000000000 ) ) ;
#2709 = CARTESIAN_POINT ( 'NONE',  ( 4.687312169500634340, -21.32903648725300272, 5.908812401261035241 ) ) ;
#2710 = CARTESIAN_POINT ( 'NONE',  ( -12.63943061533661982, -19.52125392549825733, 5.470334935344855154 ) ) ;
#2711 = CARTESIAN_POINT ( 'NONE',  ( -3.944195004867014909, -21.42722504787766624, 5.934029185143018914 ) ) ;
#2712 = VECTOR ( 'NONE', #20650, 1000.000000000000000 ) ;
#2713 = VECTOR ( 'NONE', #14659, 1000.000000000000000 ) ;
#2714 = ORIENTED_EDGE ( 'NONE', *, *, #11572, .T. ) ;
#2715 = DIRECTION ( 'NONE',  ( 1.000000000000000000, 0.000000000000000000, -0.000000000000000000 ) ) ;
#2716 = CARTESIAN_POINT ( 'NONE',  ( -5.563547257480587760, 16.00000000000000000, 1.000000000000000000 ) ) ;
#2717 = CARTESIAN_POINT ( 'NONE',  ( -13.40957725085194241, -19.25384883197511243, 6.242932005802575901 ) ) ;
#2718 = CARTESIAN_POINT ( 'NONE',  ( 13.18405858231679417, -20.79840458871652942, 2.226721677130544030 ) ) ;
#2719 = LINE ( 'NONE', #10978, #19024 ) ;
#2720 = ORIENTED_EDGE ( 'NONE', *, *, #2961, .F. ) ;
#2721 = ORIENTED_EDGE ( 'NONE', *, *, #9878, .T. ) ;
#2722 = CARTESIAN_POINT ( 'NONE',  ( 13.39169349927020569, -20.15697828685464188, 6.009339318877812808 ) ) ;
#2723 = LINE ( 'NONE', #2505, #9466 ) ;
#2724 = VERTEX_POINT ( 'NONE', #9474 ) ;
#2725 = EDGE_CURVE ( 'NONE', #4209, #16676, #1831, .T. ) ;
#2726 = CARTESIAN_POINT ( 'NONE',  ( -4.315753587183824180, -21.56469153729574018, 5.194994555241421175 ) ) ;
#2727 = ORIENTED_EDGE ( 'NONE', *, *, #6841, .F. ) ;
#2728 = CARTESIAN_POINT ( 'NONE',  ( -11.68405858231679417, -20.79840458871652942, 2.226721677130544030 ) ) ;
#2729 = AXIS2_PLACEMENT_3D ( 'NONE', #4531, #4734, #1398 ) ;
#2730 = DIRECTION ( 'NONE',  ( -0.000000000000000000, -0.000000000000000000, -1.000000000000000000 ) ) ;
#2731 = VECTOR ( 'NONE', #5285, 999.9999999999998863 ) ;
#2732 = EDGE_CURVE ( 'NONE', #4209, #12230, #4862, .T. ) ;
#2733 = PLANE ( 'NONE',  #11202 ) ;
#2734 = CARTESIAN_POINT ( 'NONE',  ( 2.309828811027716977, -9.292785183284841821, 1.668323847571005603 ) ) ;
#2735 = EDGE_CURVE ( 'NONE', #14584, #15234, #17134, .T. ) ;
#2736 = DIRECTION ( 'NONE',  ( -1.000000000000000000, 0.000000000000000000, 0.000000000000000000 ) ) ;
#2737 = CARTESIAN_POINT ( 'NONE',  ( -13.37559048950600626, -19.47018027994350220, 4.620717101209816491 ) ) ;
#2738 = CARTESIAN_POINT ( 'NONE',  ( -0.000000000000000000, 11.64110105645932691, 0.000000000000000000 ) ) ;
#2739 = CARTESIAN_POINT ( 'NONE',  ( -13.37500027835944039, -20.99998594284889464, 4.544258551573043370 ) ) ;
#2740 = FACE_OUTER_BOUND ( 'NONE', #3282, .T. ) ;
#2741 = CARTESIAN_POINT ( 'NONE',  ( 6.621558582316796837, -22.99999999999999645, 3.550687472877652073 ) ) ;
#2742 = VECTOR ( 'NONE', #6065, 1000.000000000000227 ) ;
#2743 = CARTESIAN_POINT ( 'NONE',  ( 11.40969141768317918, -21.63647391050456648, 4.520995438708348857 ) ) ;
#2744 = CARTESIAN_POINT ( 'NONE',  ( -11.59719141768317563, -22.77556120703057729, 5.229004561291656472 ) ) ;
#2745 = ORIENTED_EDGE ( 'NONE', *, *, #2735, .T. ) ;
#2746 = CARTESIAN_POINT ( 'NONE',  ( 13.37499994994395891, -19.50000252782794519, 4.474109982178703149 ) ) ;
#2747 = DIRECTION ( 'NONE',  ( 1.000000000000000000, 0.000000000000000000, 0.000000000000000000 ) ) ;
#2748 = ORIENTED_EDGE ( 'NONE', *, *, #18015, .T. ) ;
#2749 = EDGE_CURVE ( 'NONE', #4780, #5494, #20672, .T. ) ;
#2750 = VERTEX_POINT ( 'NONE', #11345 ) ;
#2751 = EDGE_CURVE ( 'NONE', #16350, #19789, #15942, .T. ) ;
#2752 = CARTESIAN_POINT ( 'NONE',  ( 10.00000000000000533, -30.00000000000000355, 1.000000000000000000 ) ) ;
#2753 = AXIS2_PLACEMENT_3D ( 'NONE', #11611, #14951, #327 ) ;
#2754 = CARTESIAN_POINT ( 'NONE',  ( -12.62888984277510218, -20.05356293986039873, 5.111704976569332537 ) ) ;
#2755 = LINE ( 'NONE', #4114, #17659 ) ;
#2756 = CARTESIAN_POINT ( 'NONE',  ( -13.85723511636018301, 4.102873376188801657, 5.986996695041598926 ) ) ;
#2757 = VECTOR ( 'NONE', #5396, 1000.000000000000000 ) ;
#2758 = CARTESIAN_POINT ( 'NONE',  ( 13.50000000000001243, -24.49999999999999289, 1.000000000000000000 ) ) ;
#2759 = DIRECTION ( 'NONE',  ( -0.000000000000000000, -0.000000000000000000, -1.000000000000000000 ) ) ;
#2760 = CARTESIAN_POINT ( 'NONE',  ( 0.000000000000000000, 10.00000000000000000, 1.000000000000000000 ) ) ;
#2761 = DIRECTION ( 'NONE',  ( -1.000000000000000000, 0.000000000000000000, 0.000000000000000000 ) ) ;
#2762 = FACE_OUTER_BOUND ( 'NONE', #2044, .T. ) ;
#2763 = CARTESIAN_POINT ( 'NONE',  ( -13.18405858231679595, -20.26807450282662160, 1.696391591240633101 ) ) ;
#2764 = CARTESIAN_POINT ( 'NONE',  ( -1.126276606324276619, -9.114917468222230923, 1.622643865078341463 ) ) ;
#2765 = ORIENTED_EDGE ( 'NONE', *, *, #9898, .T. ) ;
#2766 = CARTESIAN_POINT ( 'NONE',  ( -13.39107665282975645, -19.43812903209671461, 5.476542851584349947 ) ) ;
#2767 = CARTESIAN_POINT ( 'NONE',  ( -7.500000000000000888, -9.999999999999992895, 1.000000000000000000 ) ) ;
#2768 = CARTESIAN_POINT ( 'NONE',  ( 6.715308582316796837, -24.52099543870834708, 2.515153566944913432 ) ) ;
#2769 = CARTESIAN_POINT ( 'NONE',  ( -3.974842109207561425, -21.82955800590261575, 5.256404853634145447 ) ) ;
#2770 = ORIENTED_EDGE ( 'NONE', *, *, #13856, .F. ) ;
#2771 = CARTESIAN_POINT ( 'NONE',  ( 13.50467269799730374, -14.45152875114793467, 6.346192769197517514 ) ) ;
#2772 = CARTESIAN_POINT ( 'NONE',  ( 12.62499979224180180, -20.25001049178813162, 4.458178821399696012 ) ) ;
#2773 = ORIENTED_EDGE ( 'NONE', *, *, #18228, .F. ) ;
#2774 = ORIENTED_EDGE ( 'NONE', *, *, #1366, .F. ) ;
#2775 = VECTOR ( 'NONE', #17585, 1000.000000000000000 ) ;
#2776 = DIRECTION ( 'NONE',  ( 0.000000000000000000, 1.000000000000000000, -0.000000000000000000 ) ) ;
#2777 = EDGE_CURVE ( 'NONE', #18339, #6572, #8684, .T. ) ;
#2778 = ORIENTED_EDGE ( 'NONE', *, *, #293, .F. ) ;
#2779 = EDGE_CURVE ( 'NONE', #6813, #4981, #13015, .T. ) ;
#2780 = CARTESIAN_POINT ( 'NONE',  ( -13.87470602645761986, 4.985154336109792972, 4.583333333333296622 ) ) ;
#2781 = CARTESIAN_POINT ( 'NONE',  ( -13.50000000000000178, -0.4999999999999987232, 1.000000000000000000 ) ) ;
#2782 = EDGE_LOOP ( 'NONE', ( #13086, #10053, #16818, #6268 ) ) ;
#2783 = VECTOR ( 'NONE', #12233, 1000.000000000000000 ) ;
#2784 = CARTESIAN_POINT ( 'NONE',  ( 0.000000000000000000, 9.000000000000001776, 1.000000000000000000 ) ) ;
#2785 = FACE_BOUND ( 'NONE', #9102, .T. ) ;
#2786 = CARTESIAN_POINT ( 'NONE',  ( -16.62779268661489951, 0.000000000000000000, 1.000000000000000000 ) ) ;
#2787 = CARTESIAN_POINT ( 'NONE',  ( 3.002445346198714837, -11.66215945560911749, 2.276826493710632171 ) ) ;
#2788 = CARTESIAN_POINT ( 'NONE',  ( 0.000000000000000000, 10.00000000000000000, 1.000000000000000000 ) ) ;
#2789 = LINE ( 'NONE', #10345, #8749 ) ;
#2790 = AXIS2_PLACEMENT_3D ( 'NONE', #2726, #15374, #10785 ) ;
#2791 = EDGE_CURVE ( 'NONE', #4418, #11657, #15708, .T. ) ;
#2792 = DIRECTION ( 'NONE',  ( 0.000000000000000000, 0.000000000000000000, -1.000000000000000000 ) ) ;
#2793 = DIRECTION ( 'NONE',  ( -0.000000000000000000, 0.000000000000000000, -1.000000000000000000 ) ) ;
#2794 = DIRECTION ( 'NONE',  ( 0.000000000000000000, 1.000000000000000000, -0.000000000000000000 ) ) ;
#2795 = CARTESIAN_POINT ( 'NONE',  ( 5.878441417683177406, -22.99999999999999645, 3.449312527122335048 ) ) ;
#2796 = CARTESIAN_POINT ( 'NONE',  ( -13.05696142222617695, 1.564051822406025583, 5.955108176248398166 ) ) ;
#2797 = CARTESIAN_POINT ( 'NONE',  ( -9.621558582316795949, -22.99999999999999645, 3.550687472877652073 ) ) ;
#2798 = CARTESIAN_POINT ( 'NONE',  ( -10.09719141768317741, -23.08622137881040359, 5.979004561291654696 ) ) ;
#2799 = VERTEX_POINT ( 'NONE', #12907 ) ;
#2800 = CARTESIAN_POINT ( 'NONE',  ( 13.09533517714100093, 4.251926445620864747, 5.084080158857392284 ) ) ;
#2801 = CARTESIAN_POINT ( 'NONE',  ( 0.000000000000000000, 16.00000000000000000, 1.000000000000000000 ) ) ;
#2802 = VERTEX_POINT ( 'NONE', #13122 ) ;
#2803 = CARTESIAN_POINT ( 'NONE',  ( 6.813547257480585095, 0.000000000000000000, 1.000000000000000000 ) ) ;
#2804 = ORIENTED_EDGE ( 'NONE', *, *, #20615, .F. ) ;
#2805 = CARTESIAN_POINT ( 'NONE',  ( 1.882415164465650825, -10.11790622164856224, 2.437616430916333510 ) ) ;
#2806 = ORIENTED_EDGE ( 'NONE', *, *, #17901, .T. ) ;
#2807 = DIRECTION ( 'NONE',  ( 0.000000000000000000, -1.000000000000000000, 0.000000000000000000 ) ) ;
#2808 = LINE ( 'NONE', #1238, #13965 ) ;
#2809 = CARTESIAN_POINT ( 'NONE',  ( -2.011668220304084542, -11.03559989230542193, 2.673298498313999794 ) ) ;
#2810 = DIRECTION ( 'NONE',  ( 0.000000000000000000, 0.000000000000000000, -1.000000000000000000 ) ) ;
#2811 = DIRECTION ( 'NONE',  ( 0.000000000000000000, -1.000000000000000000, 0.000000000000000000 ) ) ;
#2812 = DIRECTION ( 'NONE',  ( 0.000000000000000000, 1.000000000000000000, -0.000000000000000000 ) ) ;
#2813 = DIRECTION ( 'NONE',  ( 1.000000000000000000, 0.000000000000000000, 0.000000000000000000 ) ) ;
#2814 = CARTESIAN_POINT ( 'NONE',  ( 8.878441417683177406, -24.50000000000000000, 3.449312527122335048 ) ) ;
#2815 = DIRECTION ( 'NONE',  ( 0.000000000000000000, 0.8660254037844364872, 0.5000000000000036637 ) ) ;
#2816 = CARTESIAN_POINT ( 'NONE',  ( -10.19094141768317563, -23.27327832286946219, 4.701595411283453707 ) ) ;
#2817 = EDGE_CURVE ( 'NONE', #14753, #13, #4762, .T. ) ;
#2818 = EDGE_LOOP ( 'NONE', ( #12637, #1943, #2745, #8128 ) ) ;
#2819 = CARTESIAN_POINT ( 'NONE',  ( 5.684058582316794173, -20.79840458871652942, 2.226721677130544030 ) ) ;
#2820 = DIRECTION ( 'NONE',  ( -0.000000000000000000, -0.000000000000000000, -1.000000000000000000 ) ) ;
#2821 = CARTESIAN_POINT ( 'NONE',  ( -13.41175265982446696, -19.14399067886409256, 6.245281310864100988 ) ) ;
#2822 = ORIENTED_EDGE ( 'NONE', *, *, #14828, .T. ) ;
#2823 = CARTESIAN_POINT ( 'NONE',  ( 9.621558582316794173, -23.74999999999999645, 3.550687472877651629 ) ) ;
#2824 = CARTESIAN_POINT ( 'NONE',  ( -12.00000000000000000, -25.49999999999998934, 4.000000000000000000 ) ) ;
#2825 = EDGE_LOOP ( 'NONE', ( #1203, #14184, #13332, #8079, #16097, #14135 ) ) ;
#2826 = ORIENTED_EDGE ( 'NONE', *, *, #17610, .T. ) ;
#2827 = CARTESIAN_POINT ( 'NONE',  ( 13.37500000000002132, -20.99999999999450395, 3.833333333368183382 ) ) ;
#2828 = PRODUCT ( 'Cast Metal _ Plastic Body Housing', 'Cast Metal _ Plastic Body Housing', '', ( #13255 ) ) ;
#2829 = DIRECTION ( 'NONE',  ( 1.000000000000000000, 0.000000000000000000, -0.000000000000000000 ) ) ;
#2830 = VERTEX_POINT ( 'NONE', #17516 ) ;
#2831 = CYLINDRICAL_SURFACE ( 'NONE', #15797, 0.4999999999999987232 ) ;
#2832 = EDGE_LOOP ( 'NONE', ( #2167, #408, #579, #12559, #3746, #13946, #2355, #2238 ) ) ;
#2833 = CARTESIAN_POINT ( 'NONE',  ( -10.55905858231679595, -20.72672167713054137, 4.701595411283463477 ) ) ;
#2834 = CARTESIAN_POINT ( 'NONE',  ( -5.433390479346035029, 4.999999999999999112, 1.000000000000000000 ) ) ;
#2835 = CARTESIAN_POINT ( 'NONE',  ( -20.00000000000000000, 0.000000000000000000, 1.000000000000000000 ) ) ;
#2836 = CARTESIAN_POINT ( 'NONE',  ( 2.747777887823422471, -9.906471667804277459, 1.825930796414880763 ) ) ;
#2837 = CARTESIAN_POINT ( 'NONE',  ( 14.99999999999999645, 3.000000000000003553, 1.000000000000000000 ) ) ;
#2838 = CARTESIAN_POINT ( 'NONE',  ( -13.09559422631463654, 4.265008428887424152, 5.017082219073495608 ) ) ;
#2839 = CARTESIAN_POINT ( 'NONE',  ( -13.40432071140796744, -19.51930407389869515, 6.223619713037471968 ) ) ;
#2840 = ADVANCED_FACE ( 'NONE', ( #6644 ), #3197, .T. ) ;
#2841 = DIRECTION ( 'NONE',  ( 0.000000000000000000, 0.000000000000000000, -1.000000000000000000 ) ) ;
#2842 = CARTESIAN_POINT ( 'NONE',  ( 5.965308582316795949, -20.97900456129165647, 3.863526089495444626 ) ) ;
#2843 = AXIS2_PLACEMENT_3D ( 'NONE', #1164, #13907, #15688 ) ;
#2844 = CARTESIAN_POINT ( 'NONE',  ( 5.597191417683179182, -22.77556120703057729, 5.229004561291655584 ) ) ;
#2845 = CARTESIAN_POINT ( 'NONE',  ( -10.47219141768317741, -23.72900456129164937, 2.724438792969417378 ) ) ;
#2846 = VERTEX_POINT ( 'NONE', #6446 ) ;
#2847 = EDGE_CURVE ( 'NONE', #17347, #16469, #19311, .T. ) ;
#2848 = CARTESIAN_POINT ( 'NONE',  ( 13.37500000000002132, -19.50000000000273559, 4.083333333315724012 ) ) ;
#2849 = EDGE_CURVE ( 'NONE', #8796, #11652, #12810, .T. ) ;
#2850 = CARTESIAN_POINT ( 'NONE',  ( -1.720709671993384093, -9.114925383610804843, 1.622645897908254753 ) ) ;
#2851 = ORIENTED_EDGE ( 'NONE', *, *, #6596, .T. ) ;
#2852 = ORIENTED_EDGE ( 'NONE', *, *, #9232, .F. ) ;
#2853 = CARTESIAN_POINT ( 'NONE',  ( -18.98630159782011262, 9.000000000000001776, 0.000000000000000000 ) ) ;
#2854 = CARTESIAN_POINT ( 'NONE',  ( -12.62599079447150885, -20.19996487918709249, 4.820256282269618886 ) ) ;
#2855 = CARTESIAN_POINT ( 'NONE',  ( -14.00000000000000000, 0.000000000000000000, 0.5000000000000000000 ) ) ;
#2856 = CARTESIAN_POINT ( 'NONE',  ( -13.87444723674697755, 4.972085455720938185, 5.163895512850782410 ) ) ;
#2857 = DIRECTION ( 'NONE',  ( -1.000000000000000000, -0.000000000000000000, -0.000000000000000000 ) ) ;
#2858 = CARTESIAN_POINT ( 'NONE',  ( 13.92791111847407848, 0.000000000000000000, 1.000000000000000000 ) ) ;
#2859 = DIRECTION ( 'NONE',  ( 0.000000000000000000, 0.000000000000000000, -1.000000000000000000 ) ) ;
#2860 = FACE_OUTER_BOUND ( 'NONE', #2405, .T. ) ;
#2861 = EDGE_CURVE ( 'NONE', #14282, #483, #9781, .T. ) ;
#2862 = DIRECTION ( 'NONE',  ( -0.000000000000000000, 0.000000000000000000, -1.000000000000000000 ) ) ;
#2863 = CARTESIAN_POINT ( 'NONE',  ( -10.27780858231679595, -19.52099543870833642, 2.413778621189609286 ) ) ;
#2864 = CARTESIAN_POINT ( 'NONE',  ( -2.808565762442263303, -10.28561894962424716, 1.923303392614186924 ) ) ;
#2865 = EDGE_LOOP ( 'NONE', ( #2826, #2049, #1487, #13747 ) ) ;
#2866 = CARTESIAN_POINT ( 'NONE',  ( -13.83770801678722329, 3.866754847752558621, 5.240062463382368030 ) ) ;
#2867 = FACE_OUTER_BOUND ( 'NONE', #15855, .T. ) ;
#2868 = CARTESIAN_POINT ( 'NONE',  ( 11.31594141768317741, -20.26807450282663225, 5.303608408759377113 ) ) ;
#2869 = CARTESIAN_POINT ( 'NONE',  ( -6.628441417683177406, -20.99999999999999645, 3.550687472877664952 ) ) ;
#2870 = ORIENTED_EDGE ( 'NONE', *, *, #2861, .F. ) ;
#2871 = CARTESIAN_POINT ( 'NONE',  ( 13.87470602645761986, 4.985154336109792972, 3.000000000000000000 ) ) ;
#2872 = LINE ( 'NONE', #4746, #1040 ) ;
#2873 = ORIENTED_EDGE ( 'NONE', *, *, #6043, .T. ) ;
#2874 = ORIENTED_EDGE ( 'NONE', *, *, #3496, .F. ) ;
#2875 = CARTESIAN_POINT ( 'NONE',  ( -11.74178095869206828, 4.999999999999999112, 0.000000000000000000 ) ) ;
#2876 = ORIENTED_EDGE ( 'NONE', *, *, #2665, .T. ) ;
#2877 = CARTESIAN_POINT ( 'NONE',  ( -13.43259567872942917, -17.34141822415733714, 5.534013032956523581 ) ) ;
#2878 = EDGE_CURVE ( 'NONE', #17965, #11811, #14580, .T. ) ;
#2879 = LINE ( 'NONE', #13951, #13466 ) ;
#2880 = ORIENTED_EDGE ( 'NONE', *, *, #13846, .F. ) ;
#2881 = CARTESIAN_POINT ( 'NONE',  ( 23.10856191738414012, 0.000000000000000000, 1.000000000000000000 ) ) ;
#2882 = CARTESIAN_POINT ( 'NONE',  ( 2.702705060698113115, -10.69015907548275379, 2.777197378435510622 ) ) ;
#2883 = LINE ( 'NONE', #12188, #6992 ) ;
#2884 = CARTESIAN_POINT ( 'NONE',  ( 3.347120161770001268, -14.10934257735911146, 2.905312006771028077 ) ) ;
#2885 = LINE ( 'NONE', #2788, #5518 ) ;
#2886 = CARTESIAN_POINT ( 'NONE',  ( 13.12512971825177033, 5.006550771716304915, 5.133277049491872468 ) ) ;
#2887 = ADVANCED_FACE ( 'NONE', ( #5076 ), #11452, .F. ) ;
#2888 = DIRECTION ( 'NONE',  ( 0.1736481776669309696, 0.9848077530122080203, 0.000000000000000000 ) ) ;
#2889 = FACE_OUTER_BOUND ( 'NONE', #9746, .T. ) ;
#2890 = ADVANCED_FACE ( 'NONE', ( #5379 ), #2234, .F. ) ;
#2891 = CARTESIAN_POINT ( 'NONE',  ( -1.561130159782011306, 0.000000000000000000, 0.000000000000000000 ) ) ;
#2892 = CARTESIAN_POINT ( 'NONE',  ( 8.690941417683177406, -22.74294823697955081, 4.171265325393542334 ) ) ;
#2893 = CARTESIAN_POINT ( 'NONE',  ( -12.64931222250080545, -19.02223276370786209, 5.512399842915133519 ) ) ;
#2894 = CARTESIAN_POINT ( 'NONE',  ( -11.49655858231679595, -22.05068747287764452, 2.499999999999999112 ) ) ;
#2895 = CARTESIAN_POINT ( 'NONE',  ( -12.06594141768317563, -23.20159541128344927, 2.226721677130534705 ) ) ;
#2896 = EDGE_CURVE ( 'NONE', #20148, #17464, #8426, .T. ) ;
#2897 = EDGE_LOOP ( 'NONE', ( #11589, #6623, #19194, #16123 ) ) ;
#2898 = CARTESIAN_POINT ( 'NONE',  ( 13.37593719518949698, -19.45267164293252193, 4.647380496992003174 ) ) ;
#2899 = CYLINDRICAL_SURFACE ( 'NONE', #2631, 10.00000000000000000 ) ;
#2900 = VERTEX_POINT ( 'NONE', #18038 ) ;
#2901 = LINE ( 'NONE', #2803, #17321 ) ;
#2902 = ORIENTED_EDGE ( 'NONE', *, *, #20416, .F. ) ;
#2903 = CARTESIAN_POINT ( 'NONE',  ( 1.797604806073912709, -9.120796646272857799, 2.374153755450133740 ) ) ;
#2904 = AXIS2_PLACEMENT_3D ( 'NONE', #3090, #1823, #1514 ) ;
#2905 = EDGE_CURVE ( 'NONE', #16449, #11562, #2138, .T. ) ;
#2906 = ORIENTED_EDGE ( 'NONE', *, *, #11391, .T. ) ;
#2907 = PLANE ( 'NONE',  #10323 ) ;
#2908 = LINE ( 'NONE', #20696, #16000 ) ;
#2909 = VECTOR ( 'NONE', #5961, 1000.000000000000000 ) ;
#2910 = CARTESIAN_POINT ( 'NONE',  ( -1.882415164465650825, -10.11790622164856224, 2.437616430916333510 ) ) ;
#2911 = CARTESIAN_POINT ( 'NONE',  ( 27.00000000000000000, 0.000000000000000000, 0.000000000000000000 ) ) ;
#2912 = DIRECTION ( 'NONE',  ( 0.000000000000000000, -1.000000000000000000, 0.000000000000000000 ) ) ;
#2913 = CIRCLE ( 'NONE', #13920, 2.999999999999999112 ) ;
#2914 = CARTESIAN_POINT ( 'NONE',  ( 4.659691417683177406, -22.98484643305507191, 0.9790045612916508100 ) ) ;
#2915 = SURFACE_STYLE_FILL_AREA ( #9399 ) ;
#2916 = CARTESIAN_POINT ( 'NONE',  ( -10.75344141768317741, -21.94931252712233061, 1.749999999999998446 ) ) ;
#2917 = VERTEX_POINT ( 'NONE', #2338 ) ;
#2918 = CARTESIAN_POINT ( 'NONE',  ( 6.902808582316793284, -22.77556120703056308, 1.770995438708339975 ) ) ;
#2919 = LINE ( 'NONE', #4586, #17101 ) ;
#2920 = CARTESIAN_POINT ( 'NONE',  ( -12.65346245025441263, -19.56264626215117275, 6.228892365149262922 ) ) ;
#2921 = ORIENTED_EDGE ( 'NONE', *, *, #1772, .F. ) ;
#2922 = CARTESIAN_POINT ( 'NONE',  ( 7.559058582316794173, -20.72672167713054137, 4.701595411283463477 ) ) ;
#2923 = CARTESIAN_POINT ( 'NONE',  ( -14.99999999999998401, -25.49999999999999645, 4.000000000000000000 ) ) ;
#2924 = VERTEX_POINT ( 'NONE', #11855 ) ;
#2925 = CARTESIAN_POINT ( 'NONE',  ( 13.85956729540471066, 3.470648417939721231, 6.731609435864099211 ) ) ;
#2926 = CARTESIAN_POINT ( 'NONE',  ( 0.000000000000000000, 9.000000000000001776, 1.000000000000000000 ) ) ;
#2927 = EDGE_LOOP ( 'NONE', ( #15215, #19844, #18600, #10179 ) ) ;
#2928 = EDGE_CURVE ( 'NONE', #7935, #20454, #567, .T. ) ;
#2929 = DIRECTION ( 'NONE',  ( -0.9848077530122082424, -0.1736481776669295263, 0.000000000000000000 ) ) ;
#2930 = VERTEX_POINT ( 'NONE', #8732 ) ;
#2931 = CARTESIAN_POINT ( 'NONE',  ( -9.809058582316794173, -23.27327832286945153, 2.298404588716537411 ) ) ;
#2932 = CARTESIAN_POINT ( 'NONE',  ( 13.87406079471522347, 4.952570133121557028, 5.260711232101737522 ) ) ;
#2933 = CARTESIAN_POINT ( 'NONE',  ( -13.17791111847408025, 9.000000000000001776, 0.000000000000000000 ) ) ;
#2934 = CARTESIAN_POINT ( 'NONE',  ( 3.521144778809589315, -10.09312707791070096, 2.066482617302010105 ) ) ;
#2935 = LINE ( 'NONE', #15691, #2009 ) ;
#2936 = CARTESIAN_POINT ( 'NONE',  ( -13.37893135632597819, -19.30146650553847465, 4.738802066438188909 ) ) ;
#2937 = CARTESIAN_POINT ( 'NONE',  ( 9.059058582316794173, -20.72672167713054137, 4.701595411283463477 ) ) ;
#2938 = CARTESIAN_POINT ( 'NONE',  ( -13.90439735423812273, 5.734566389025032684, 3.666666666666500873 ) ) ;
#2939 = CARTESIAN_POINT ( 'NONE',  ( 9.830951894845298966, -2.500000000000047518, 7.000000000000000000 ) ) ;
#2940 = CARTESIAN_POINT ( 'NONE',  ( 9.527808582316792396, -23.72900456129165647, 4.275561207030568411 ) ) ;
#2941 = CARTESIAN_POINT ( 'NONE',  ( 6.628441417683177406, -20.99999999999999645, 3.550687472877664952 ) ) ;
#2942 = CARTESIAN_POINT ( 'NONE',  ( -7.184058582316794173, -20.79840458871652942, 2.226721677130544030 ) ) ;
#2943 = CIRCLE ( 'NONE', #10308, 10.00000000000000000 ) ;
#2944 = VERTEX_POINT ( 'NONE', #8520 ) ;
#2945 = CARTESIAN_POINT ( 'NONE',  ( 13.09560264576187905, 4.265433610975056133, 4.583333333333295734 ) ) ;
#2946 = FACE_OUTER_BOUND ( 'NONE', #3035, .T. ) ;
#2947 = ORIENTED_EDGE ( 'NONE', *, *, #4936, .T. ) ;
#2948 = UNCERTAINTY_MEASURE_WITH_UNIT (LENGTH_MEASURE( 1.000000000000000082E-05 ), #5234, 'distance_accuracy_value', 'NONE');
#2949 = ORIENTED_EDGE ( 'NONE', *, *, #3053, .F. ) ;
#2950 = LINE ( 'NONE', #14229, #6777 ) ;
#2951 = EDGE_CURVE ( 'NONE', #13563, #8562, #3701, .T. ) ;
#2952 = CARTESIAN_POINT ( 'NONE',  ( -12.63465172146706728, -19.76258806590802664, 5.372658420469845986 ) ) ;
#2953 = AXIS2_PLACEMENT_3D ( 'NONE', #9282, #3119, #14399 ) ;
#2954 = CARTESIAN_POINT ( 'NONE',  ( -3.302240162463773832, -9.695145533921818881, 2.714273006325518711 ) ) ;
#2955 = CARTESIAN_POINT ( 'NONE',  ( -13.85223456079946303, 3.850345320370711644, 5.989742199623227847 ) ) ;
#2956 = AXIS2_PLACEMENT_3D ( 'NONE', #8491, #18002, #5454 ) ;
#2957 = EDGE_CURVE ( 'NONE', #3619, #886, #14033, .T. ) ;
#2958 = CARTESIAN_POINT ( 'NONE',  ( 30.80549002841696904, 5.431839045955454637, 1.000000000000000000 ) ) ;
#2959 = CARTESIAN_POINT ( 'NONE',  ( 0.000000000000000000, 4.999999999999999112, 1.000000000000000000 ) ) ;
#2960 = CYLINDRICAL_SURFACE ( 'NONE', #3344, 1.000000000000002665 ) ;
#2961 = EDGE_CURVE ( 'NONE', #10855, #3441, #20405, .T. ) ;
#2962 = CARTESIAN_POINT ( 'NONE',  ( -5.433390479346035029, 9.000000000000001776, 0.000000000000000000 ) ) ;
#2963 = CARTESIAN_POINT ( 'NONE',  ( 12.62499999999998224, -20.25000000000006395, 4.416666666666681174 ) ) ;
#2964 = AXIS2_PLACEMENT_3D ( 'NONE', #6145, #12415, #12515 ) ;
#2965 = CARTESIAN_POINT ( 'NONE',  ( -6.059058582316795949, -20.19639159124062999, 5.231925497173373074 ) ) ;
#2966 = CARTESIAN_POINT ( 'NONE',  ( -0.2815691515810352374, -9.864917468222230923, 1.622643865078524428 ) ) ;
#2967 = VERTEX_POINT ( 'NONE', #1797 ) ;
#2968 = CARTESIAN_POINT ( 'NONE',  ( -13.37499999999998401, -20.24999999999998934, 2.439580858552613751 ) ) ;
#2969 = CARTESIAN_POINT ( 'NONE',  ( 0.000000000000000000, 0.000000000000000000, 1.000000000000000000 ) ) ;
#2970 = CARTESIAN_POINT ( 'NONE',  ( 5.496558582316795949, -22.05068747287764452, 0.9999999999999978906 ) ) ;
#2971 = CARTESIAN_POINT ( 'NONE',  ( -4.378441417683176518, -22.99999999999999645, 3.449312527122335048 ) ) ;
#2972 = EDGE_LOOP ( 'NONE', ( #18261, #1789, #16206, #1304 ) ) ;
#2973 = CARTESIAN_POINT ( 'NONE',  ( 13.41475008041063433, -18.99262093926051520, 6.248536519197435801 ) ) ;
#2974 = CARTESIAN_POINT ( 'NONE',  ( -11.99999999999999645, -26.49999999999998934, 4.000000000000000000 ) ) ;
#2975 = CLOSED_SHELL ( 'NONE', ( #7499, #2277, #12051, #3012, #15989, #12541, #13547, #6853, #11164, #7868, #2890, #11870, #15055, #10182, #4383, #2567, #20489, #20113, #3888, #8779, #19760, #96, #8888, #13109, #6176, #12353, #5128, #20122, #13726, #18973, #6075, #4693, #7047, #10452, #2241, #6249, #12341, #5066, #15667, #16188, #17583, #19337, #5792, #3365, #20058, #2840, #15239, #6192, #3221, #20166, #16187, #13179, #11921, #2028, #18117, #4162, #3329, #19477, #14418, #9146, #13684, #9283, #17274, #11531, #15888, #15805, #9396, #20547, #1692, #17090, #4502, #12352, #15496, #15274, #8624, #15868, #10049, #14227, #19010, #20582, #10699, #9988, #10763, #9212, #18575, #14499, #758, #6487, #8773, #11011, #17860, #3679, #20006, #12084, #18058, #18480, #18817, #13181, #5716, #9299, #16222, #12729, #15373, #19384, #17874, #7187, #18926, #15924, #10371, #3115, #8774, #4527, #14986, #19902, #19712, #15773, #1450, #8140, #18315, #17029, #18698, #9732, #13808, #2459, #8251, #5820, #19453, #15121, #16508, #11804, #9007, #18742, #19854, #17348, #5578, #19942, #18438, #3515, #19866, #591, #18371, #2364, #14884, #10136, #2887, #12593, #12880, #6816 ) ) ;
#2976 = ORIENTED_EDGE ( 'NONE', *, *, #20430, .F. ) ;
#2977 = VECTOR ( 'NONE', #14711, 1000.000000000000000 ) ;
#2978 = ORIENTED_EDGE ( 'NONE', *, *, #12919, .F. ) ;
#2979 = CARTESIAN_POINT ( 'NONE',  ( 0.000000000000000000, 10.00000000000000000, 1.000000000000000000 ) ) ;
#2980 = CIRCLE ( 'NONE', #20024, 0.4999999999999987232 ) ;
#2981 = EDGE_LOOP ( 'NONE', ( #14500, #6094, #12941, #13436 ) ) ;
#2982 = LINE ( 'NONE', #9869, #6091 ) ;
#2983 = EDGE_CURVE ( 'NONE', #15823, #9991, #11518, .T. ) ;
#2984 = CARTESIAN_POINT ( 'NONE',  ( 0.5631383031621635116, -9.114917468222230923, 2.372643865078341019 ) ) ;
#2985 = ORIENTED_EDGE ( 'NONE', *, *, #1362, .F. ) ;
#2986 = DIRECTION ( 'NONE',  ( -1.000000000000000000, -0.000000000000000000, -0.000000000000000000 ) ) ;
#2987 = CARTESIAN_POINT ( 'NONE',  ( 2.616536356806028696, -10.07836329504444706, 2.620076000170431296 ) ) ;
#2988 = AXIS2_PLACEMENT_3D ( 'NONE', #3732, #13144, #11263 ) ;
#2989 = CARTESIAN_POINT ( 'NONE',  ( -12.00000000000000000, -25.49999999999998934, 4.000000000000000000 ) ) ;
#2990 = CARTESIAN_POINT ( 'NONE',  ( 1.337453470010121714, -8.364917468222230923, 1.622643865078341907 ) ) ;
#2991 = LINE ( 'NONE', #1423, #7183 ) ;
#2992 = CARTESIAN_POINT ( 'NONE',  ( 11.00000000000000000, -19.49999999999999645, 4.000000000000000000 ) ) ;
#2993 = VECTOR ( 'NONE', #3390, 1000.000000000000000 ) ;
#2994 = CARTESIAN_POINT ( 'NONE',  ( -27.00000000000000000, 0.000000000000000000, 1.000000000000000000 ) ) ;
#2995 = DIRECTION ( 'NONE',  ( -1.000000000000000000, -0.000000000000000000, -0.000000000000000000 ) ) ;
#2996 = LINE ( 'NONE', #4560, #4660 ) ;
#2997 = CARTESIAN_POINT ( 'NONE',  ( 4.753441417683176518, -21.94931252712233061, 2.499999999999999112 ) ) ;
#2998 = CARTESIAN_POINT ( 'NONE',  ( -13.08573665985359824, 3.017201322601628100, 5.986358176248492313 ) ) ;
#2999 = EDGE_CURVE ( 'NONE', #868, #11896, #3164, .T. ) ;
#3000 = CARTESIAN_POINT ( 'NONE',  ( -10.37155858231679595, -20.99999999999999645, 3.449312527122348371 ) ) ;
#3001 = CARTESIAN_POINT ( 'NONE',  ( -12.62844141768317741, -20.24999999999999289, 3.550687472877664952 ) ) ;
#3002 = ORIENTED_EDGE ( 'NONE', *, *, #12679, .T. ) ;
#3003 = CARTESIAN_POINT ( 'NONE',  ( 13.09494140422671471, 4.232040913449062636, 5.131376921800749003 ) ) ;
#3004 = FACE_OUTER_BOUND ( 'NONE', #7410, .T. ) ;
#3005 = ORIENTED_EDGE ( 'NONE', *, *, #3962, .T. ) ;
#3006 = CARTESIAN_POINT ( 'NONE',  ( 2.601332995093193379, -9.970398767539743190, 2.592349323443654097 ) ) ;
#3007 = ORIENTED_EDGE ( 'NONE', *, *, #5387, .F. ) ;
#3008 = CARTESIAN_POINT ( 'NONE',  ( 2.702705060698113115, -10.69015907548275379, 2.777197378435510622 ) ) ;
#3009 = VECTOR ( 'NONE', #1517, 1000.000000000000000 ) ;
#3010 = EDGE_CURVE ( 'NONE', #11512, #8225, #8280, .T. ) ;
#3011 = PRESENTATION_LAYER_ASSIGNMENT (  '', '', ( #2005 ) ) ;
#3012 = ADVANCED_FACE ( 'NONE', ( #17695, #19489, #17900, #21, #16022 ), #2002, .F. ) ;
#3013 = ORIENTED_EDGE ( 'NONE', *, *, #13364, .F. ) ;
#3014 = CARTESIAN_POINT ( 'NONE',  ( 8.128441417683175629, -20.24999999999999289, 3.550687472877664952 ) ) ;
#3015 = FACE_OUTER_BOUND ( 'NONE', #2433, .T. ) ;
#3016 = AXIS2_PLACEMENT_3D ( 'NONE', #2394, #10656, #18716 ) ;
#3017 = CARTESIAN_POINT ( 'NONE',  ( -1.865667289525601680, -9.999006358835732300, 2.407080570882605297 ) ) ;
#3018 = DIRECTION ( 'NONE',  ( 0.000000000000000000, -0.000000000000000000, 1.000000000000000000 ) ) ;
#3019 = CARTESIAN_POINT ( 'NONE',  ( 14.50000000000000000, -23.00000000000001421, 1.000000000000000000 ) ) ;
#3020 = CARTESIAN_POINT ( 'NONE',  ( 14.50000000000000000, -20.99999999999998934, 4.000000000000000000 ) ) ;
#3021 = VECTOR ( 'NONE', #1650, 1000.000000000000227 ) ;
#3022 = CARTESIAN_POINT ( 'NONE',  ( 9.253441417683177406, -21.94931252712233061, 0.9999999999999978906 ) ) ;
#3023 = DIRECTION ( 'NONE',  ( 0.000000000000000000, -0.000000000000000000, 1.000000000000000000 ) ) ;
#3024 = CARTESIAN_POINT ( 'NONE',  ( -10.84719141768317563, -21.22443879296941915, 1.770995438708345748 ) ) ;
#3025 = ORIENTED_EDGE ( 'NONE', *, *, #14321, .F. ) ;
#3026 = CARTESIAN_POINT ( 'NONE',  ( 9.809058582316794173, -23.27327832286945153, 2.298404588716537411 ) ) ;
#3027 = DIRECTION ( 'NONE',  ( -0.000000000000000000, 0.000000000000000000, -1.000000000000000000 ) ) ;
#3028 = CARTESIAN_POINT ( 'NONE',  ( -13.90439706815434739, 5.734551941788608609, 5.045486763335835789 ) ) ;
#3029 = VERTEX_POINT ( 'NONE', #17803 ) ;
#3030 = AXIS2_PLACEMENT_3D ( 'NONE', #7133, #4089, #15267 ) ;
#3031 = CARTESIAN_POINT ( 'NONE',  ( 6.434058582316794173, -23.20159541128345992, 4.773278322869455970 ) ) ;
#3032 = CARTESIAN_POINT ( 'NONE',  ( -14.56494360078803396, 10.00000000000000000, 1.000000000000000000 ) ) ;
#3033 = ORIENTED_EDGE ( 'NONE', *, *, #12553, .T. ) ;
#3034 = CARTESIAN_POINT ( 'NONE',  ( 11.00000000000000000, -23.83493649053891517, 5.249999999999999112 ) ) ;
#3035 = EDGE_LOOP ( 'NONE', ( #2082, #7589, #3333, #14527 ) ) ;
#3036 = B_SPLINE_CURVE_WITH_KNOTS ( 'NONE', 3,
 ( #1834, #9477, #15746, #13019, #4968, #164, #20675, #1428, #6547, #4865 ),
 .UNSPECIFIED., .F., .F.,
 ( 4, 2, 2, 2, 4 ),
 ( 0.000000000000000000, 0.0002944886444448786226, 0.0005889772888897572452, 0.0008834659333346358678, 0.001177954577779514490 ),
 .UNSPECIFIED. ) ;
#3037 = LINE ( 'NONE', #17463, #7464 ) ;
#3038 = EDGE_CURVE ( 'NONE', #2127, #18601, #16130, .T. ) ;
#3039 = ORIENTED_EDGE ( 'NONE', *, *, #15226, .F. ) ;
#3040 = CARTESIAN_POINT ( 'NONE',  ( -8.684058582316794173, -20.79840458871652942, 2.226721677130544030 ) ) ;
#3041 = CARTESIAN_POINT ( 'NONE',  ( 12.62499999999998224, -20.24999999999991829, 4.333333333333343695 ) ) ;
#3042 =( GEOMETRIC_REPRESENTATION_CONTEXT ( 3 ) GLOBAL_UNCERTAINTY_ASSIGNED_CONTEXT ( ( #2326 ) ) GLOBAL_UNIT_ASSIGNED_CONTEXT ( ( #12848, #16301, #17560 ) ) REPRESENTATION_CONTEXT ( 'NONE', 'WORKASPACE' ) );
#3043 = VECTOR ( 'NONE', #9834, 1000.000000000000000 ) ;
#3044 = FACE_OUTER_BOUND ( 'NONE', #11441, .T. ) ;
#3045 = CARTESIAN_POINT ( 'NONE',  ( 0.9854920305337622199, -9.864917468222230923, 1.622643865078341907 ) ) ;
#3046 = VECTOR ( 'NONE', #4131, 1000.000000000000000 ) ;
#3047 = VECTOR ( 'NONE', #16037, 1000.000000000000114 ) ;
#3048 = CIRCLE ( 'NONE', #20424, 10.00000000000000000 ) ;
#3049 = DIRECTION ( 'NONE',  ( -0.000000000000000000, -0.000000000000000000, -1.000000000000000000 ) ) ;
#3050 = CARTESIAN_POINT ( 'NONE',  ( -13.84051394328565365, 4.008454135954084840, 5.243107695145536873 ) ) ;
#3051 = CARTESIAN_POINT ( 'NONE',  ( 5.121558582316794173, -23.74999999999999645, 3.550687472877651629 ) ) ;
#3052 = CARTESIAN_POINT ( 'NONE',  ( -12.62499999999998401, -20.99999999999999645, 3.146526952850934755 ) ) ;
#3053 = EDGE_CURVE ( 'NONE', #5903, #4592, #11310, .T. ) ;
#3054 = DIRECTION ( 'NONE',  ( -0.000000000000000000, -0.000000000000000000, -1.000000000000000000 ) ) ;
#3055 = LINE ( 'NONE', #15801, #10085 ) ;
#3056 = CARTESIAN_POINT ( 'NONE',  ( 4.659691417683177406, -22.36352608949543352, 2.479004561291652031 ) ) ;
#3057 = CARTESIAN_POINT ( 'NONE',  ( -7.371558582316794173, -20.24999999999999289, 3.449312527122348371 ) ) ;
#3058 = VERTEX_POINT ( 'NONE', #6514 ) ;
#3059 = CARTESIAN_POINT ( 'NONE',  ( 13.37930517931174634, -19.28258844475809042, 4.742233558278135419 ) ) ;
#3060 = CARTESIAN_POINT ( 'NONE',  ( -1.652577328807104839, -9.114908150887895744, 1.622641472200749835 ) ) ;
#3061 = VERTEX_POINT ( 'NONE', #14652 ) ;
#3062 = VERTEX_POINT ( 'NONE', #333 ) ;
#3063 = LINE ( 'NONE', #11211, #4769 ) ;
#3064 = PRODUCT_RELATED_PRODUCT_CATEGORY ( 'part', '', ( #19212 ) ) ;
#3065 = DIRECTION ( 'NONE',  ( -1.000000000000000000, -0.000000000000000000, -0.000000000000000000 ) ) ;
#3066 = CARTESIAN_POINT ( 'NONE',  ( -1.787053415088318609, -8.367039355952382351, 2.373188808236395886 ) ) ;
#3067 = CARTESIAN_POINT ( 'NONE',  ( 12.00000000000000178, -26.50000000000000355, 4.000000000000000000 ) ) ;
#3068 = DIRECTION ( 'NONE',  ( -0.000000000000000000, -0.000000000000000000, -1.000000000000000000 ) ) ;
#3069 = DIRECTION ( 'NONE',  ( 0.4999999999999950040, -0.8660254037844415942, 0.000000000000000000 ) ) ;
#3070 = CARTESIAN_POINT ( 'NONE',  ( 10.37155858231679417, -20.24999999999999289, 3.449312527122348371 ) ) ;
#3071 = CARTESIAN_POINT ( 'NONE',  ( 15.06494360078803041, 0.000000000000000000, 0.000000000000000000 ) ) ;
#3072 = CARTESIAN_POINT ( 'NONE',  ( 12.68302225826488616, -18.06987595762608478, 6.282912912489355683 ) ) ;
#3073 = AXIS2_PLACEMENT_3D ( 'NONE', #20214, #7549, #12145 ) ;
#3074 = CARTESIAN_POINT ( 'NONE',  ( -4.717959273841179524, -21.63341328858655999, 5.993595146365859883 ) ) ;
#3075 = CARTESIAN_POINT ( 'NONE',  ( -1.710927537542899612, -9.866086492083725901, 2.372944093759576933 ) ) ;
#3076 = ORIENTED_EDGE ( 'NONE', *, *, #16276, .F. ) ;
#3077 = CARTESIAN_POINT ( 'NONE',  ( -13.84439157666246878, 4.204274621457510186, 5.123803251657143676 ) ) ;
#3078 = DIRECTION ( 'NONE',  ( 0.000000000000000000, -0.1264857625231113059, -0.9919684228235025047 ) ) ;
#3079 = EDGE_CURVE ( 'NONE', #7127, #7382, #17721, .T. ) ;
#3080 = CARTESIAN_POINT ( 'NONE',  ( 3.944195004867014909, -21.42722504787766624, 5.934029185143018914 ) ) ;
#3081 = CARTESIAN_POINT ( 'NONE',  ( -11.40280858231679595, -22.46490103525074034, 2.520995438708341307 ) ) ;
#3082 = ORIENTED_EDGE ( 'NONE', *, *, #8366, .T. ) ;
#3083 = CARTESIAN_POINT ( 'NONE',  ( 13.87444723674697755, 4.972085455720938185, 5.163895512850782410 ) ) ;
#3084 = CARTESIAN_POINT ( 'NONE',  ( 12.63819864697926754, -19.58346832754827105, 5.450273968536036406 ) ) ;
#3085 = DIRECTION ( 'NONE',  ( -1.000000000000000000, -0.000000000000000000, -0.000000000000000000 ) ) ;
#3086 = ORIENTED_EDGE ( 'NONE', *, *, #1166, .T. ) ;
#3087 = ORIENTED_EDGE ( 'NONE', *, *, #10578, .T. ) ;
#3088 = DIRECTION ( 'NONE',  ( 1.000000000000000000, 0.000000000000000000, 0.000000000000000000 ) ) ;
#3089 = VECTOR ( 'NONE', #8023, 1000.000000000000000 ) ;
#3090 = CARTESIAN_POINT ( 'NONE',  ( 0.000000000000000000, 0.000000000000000000, 4.000000000000000000 ) ) ;
#3091 = ORIENTED_EDGE ( 'NONE', *, *, #8983, .T. ) ;
#3092 = CARTESIAN_POINT ( 'NONE',  ( 0.000000000000000000, 9.000000000000001776, 0.000000000000000000 ) ) ;
#3093 = CARTESIAN_POINT ( 'NONE',  ( -15.49999999999999822, -22.99999999999999289, 4.000000000000000000 ) ) ;
#3094 = DIRECTION ( 'NONE',  ( 0.000000000000000000, 1.000000000000000000, 0.000000000000000000 ) ) ;
#3095 = CARTESIAN_POINT ( 'NONE',  ( 1.513434189748285918, -8.364917468222230923, 1.622643865078341907 ) ) ;
#3096 = CARTESIAN_POINT ( 'NONE',  ( -27.50000000000000355, 3.000000000000000888, 1.000000000000000000 ) ) ;
#3097 = DIRECTION ( 'NONE',  ( 1.000000000000000000, -0.000000000000000000, 0.000000000000000000 ) ) ;
#3098 = DIRECTION ( 'NONE',  ( -1.000000000000000000, -0.000000000000000000, -0.000000000000000000 ) ) ;
#3099 = CARTESIAN_POINT ( 'NONE',  ( 0.000000000000000000, 4.999999999999999112, 1.000000000000000000 ) ) ;
#3100 = CARTESIAN_POINT ( 'NONE',  ( 0.000000000000000000, 0.000000000000000000, 1.000000000000000000 ) ) ;
#3101 = CARTESIAN_POINT ( 'NONE',  ( 6.065941417683177406, -22.67126532539353789, 2.757051763020445634 ) ) ;
#3102 = CARTESIAN_POINT ( 'NONE',  ( -13.10557919622060652, 4.019249409169220577, 6.007898877577752650 ) ) ;
#3103 = CARTESIAN_POINT ( 'NONE',  ( -9.996558582316795949, -22.05068747287764452, 2.499999999999999112 ) ) ;
#3104 = CIRCLE ( 'NONE', #14784, 10.00000000000000000 ) ;
#3105 = EDGE_CURVE ( 'NONE', #13135, #11513, #19380, .T. ) ;
#3106 = CARTESIAN_POINT ( 'NONE',  ( -10.47219141768317563, -23.72900456129165292, 2.724438792969417822 ) ) ;
#3107 = ORIENTED_EDGE ( 'NONE', *, *, #16512, .F. ) ;
#3108 = CARTESIAN_POINT ( 'NONE',  ( 13.09206359972826661, 4.086711786274932479, 5.245812454509717782 ) ) ;
#3109 = LINE ( 'NONE', #7816, #19369 ) ;
#3110 = EDGE_LOOP ( 'NONE', ( #5314, #11766, #10025, #5704 ) ) ;
#3111 = CARTESIAN_POINT ( 'NONE',  ( 15.50000000000000178, -20.99999999999999645, 4.000000000000000000 ) ) ;
#3112 = ORIENTED_EDGE ( 'NONE', *, *, #2479, .T. ) ;
#3113 = CARTESIAN_POINT ( 'NONE',  ( 15.50000000000000178, -23.00000000000000711, 4.000000000000000000 ) ) ;
#3114 = EDGE_CURVE ( 'NONE', #12054, #5420, #19069, .T. ) ;
#3115 = ADVANCED_FACE ( 'NONE', ( #3367 ), #8388, .T. ) ;
#3116 = ORIENTED_EDGE ( 'NONE', *, *, #18821, .T. ) ;
#3117 = CARTESIAN_POINT ( 'NONE',  ( 8.972191417683177406, -23.72900456129164937, 2.724438792969417378 ) ) ;
#3118 = AXIS2_PLACEMENT_3D ( 'NONE', #17355, #11282, #17665 ) ;
#3119 = DIRECTION ( 'NONE',  ( -1.000000000000000000, 0.000000000000000000, 0.000000000000000000 ) ) ;
#3120 = CARTESIAN_POINT ( 'NONE',  ( -2.436080212393455735, -9.483920418190111334, 2.467411194204634839 ) ) ;
#3121 = CARTESIAN_POINT ( 'NONE',  ( -13.49999999999998401, -25.49999999999999645, 4.000000000000000000 ) ) ;
#3122 = CARTESIAN_POINT ( 'NONE',  ( -4.000000000000000000, -12.50000000000000000, 3.464723819589916154 ) ) ;
#3123 = CARTESIAN_POINT ( 'NONE',  ( -14.49999999999998579, -19.49999999999999645, 4.000000000000000000 ) ) ;
#3124 = CARTESIAN_POINT ( 'NONE',  ( 7.378441417683177406, -24.50000000000000000, 3.449312527122335048 ) ) ;
#3125 = LINE ( 'NONE', #11076, #13866 ) ;
#3126 = CARTESIAN_POINT ( 'NONE',  ( -8.503441417683177406, -22.05068747287765873, 5.250000000000000888 ) ) ;
#3127 = EDGE_CURVE ( 'NONE', #12822, #9362, #11212, .T. ) ;
#3128 = ORIENTED_EDGE ( 'NONE', *, *, #7691, .T. ) ;
#3129 = CARTESIAN_POINT ( 'NONE',  ( 5.496558582316794173, -22.05068747287764452, 1.749999999999998446 ) ) ;
#3130 = CARTESIAN_POINT ( 'NONE',  ( -13.90326467458556969, 5.677366066573198644, 5.457668599364335904 ) ) ;
#3131 = ORIENTED_EDGE ( 'NONE', *, *, #7199, .F. ) ;
#3132 = CARTESIAN_POINT ( 'NONE',  ( 4.717959273841178636, -21.72818306014730183, 5.243595146365860771 ) ) ;
#3133 = DIRECTION ( 'NONE',  ( 1.000000000000000000, 6.938893903907232322E-16, 0.000000000000000000 ) ) ;
#3134 = ORIENTED_EDGE ( 'NONE', *, *, #2318, .T. ) ;
#3135 = DIRECTION ( 'NONE',  ( 0.000000000000000000, 1.000000000000000000, -0.000000000000000000 ) ) ;
#3136 = SURFACE_STYLE_FILL_AREA ( #11087 ) ;
#3137 = ORIENTED_EDGE ( 'NONE', *, *, #6636, .T. ) ;
#3138 = CARTESIAN_POINT ( 'NONE',  ( -1.734723475976795735E-14, 10.00000000000004619, 0.000000000000000000 ) ) ;
#3139 = AXIS2_PLACEMENT_3D ( 'NONE', #10187, #16557, #2232 ) ;
#3140 = VERTEX_POINT ( 'NONE', #6610 ) ;
#3141 = CARTESIAN_POINT ( 'NONE',  ( -5.777808582316794173, -20.27099543870833642, 2.724438792969431589 ) ) ;
#3142 = CARTESIAN_POINT ( 'NONE',  ( 12.62599079447150885, -20.19996487918709249, 4.820256282269618886 ) ) ;
#3143 = VECTOR ( 'NONE', #11902, 1000.000000000000000 ) ;
#3144 = CARTESIAN_POINT ( 'NONE',  ( -4.000000000000000000, -8.500000000000000000, 2.392927049865408495 ) ) ;
#3145 = CARTESIAN_POINT ( 'NONE',  ( 0.000000000000000000, -9.864917468222230923, 1.622643865078341241 ) ) ;
#3146 = LINE ( 'NONE', #12647, #5008 ) ;
#3147 = CARTESIAN_POINT ( 'NONE',  ( -13.84501469867365131, 4.235742283194553259, 3.333333333332063386 ) ) ;
#3148 = CARTESIAN_POINT ( 'NONE',  ( 9.527808582316792396, -23.72900456129165647, 4.275561207030568411 ) ) ;
#3149 = CARTESIAN_POINT ( 'NONE',  ( -12.62500000000002132, -21.00000000000274269, 4.083333333315724012 ) ) ;
#3150 = EDGE_CURVE ( 'NONE', #20018, #4438, #17587, .T. ) ;
#3151 = ADVANCED_FACE ( 'NONE', ( #9748 ), #223, .T. ) ;
#3152 = FACE_OUTER_BOUND ( 'NONE', #4829, .T. ) ;
#3153 = CARTESIAN_POINT ( 'NONE',  ( -5.965308582316795949, -19.47900456129164937, 4.484846433055089676 ) ) ;
#3154 = CARTESIAN_POINT ( 'NONE',  ( 0.000000000000000000, 9.000000000000001776, 1.000000000000000000 ) ) ;
#3155 = CARTESIAN_POINT ( 'NONE',  ( 5.784691417683178294, -23.02099543870834353, 3.863526089495429972 ) ) ;
#3156 = CARTESIAN_POINT ( 'NONE',  ( -4.687312169500632564, -21.51559725698341197, 5.182386163300427562 ) ) ;
#3157 = ORIENTED_EDGE ( 'NONE', *, *, #9533, .F. ) ;
#3158 = CARTESIAN_POINT ( 'NONE',  ( 13.84311479963346869, 4.139797381492562600, 5.195993353439945395 ) ) ;
#3159 = CARTESIAN_POINT ( 'NONE',  ( -5.933390479346035029, 0.000000000000000000, 1.000000000000000000 ) ) ;
#3160 = ORIENTED_EDGE ( 'NONE', *, *, #1682, .F. ) ;
#3161 = PRODUCT_DEFINITION_CONTEXT ( 'detailed design', #17226, 'design' ) ;
#3162 = ORIENTED_EDGE ( 'NONE', *, *, #9798, .F. ) ;
#3163 = CARTESIAN_POINT ( 'NONE',  ( -7.500000000000000000, -20.29006350946107418, 5.466506350946110260 ) ) ;
#3164 = LINE ( 'NONE', #6409, #13702 ) ;
#3165 = EDGE_CURVE ( 'NONE', #15422, #10048, #5700, .T. ) ;
#3166 = CARTESIAN_POINT ( 'NONE',  ( -13.12529397354238192, 5.014845663890295846, 4.333333333333374782 ) ) ;
#3167 = CARTESIAN_POINT ( 'NONE',  ( -1.407845757905374695, -8.364917468222230923, 2.372643865078341019 ) ) ;
#3168 = CARTESIAN_POINT ( 'NONE',  ( -2.187849085826861550, 16.00000000000000000, 1.000000000000000000 ) ) ;
#3169 = CARTESIAN_POINT ( 'NONE',  ( 2.786182376113650605, -10.12667130264514626, 1.882483419865550900 ) ) ;
#3170 = CARTESIAN_POINT ( 'NONE',  ( -12.72125031657057015, -15.38935901321805133, 5.590524842915047365 ) ) ;
#3171 = CARTESIAN_POINT ( 'NONE',  ( 13.37327929115833669, -20.24999999707183207, 3.449077790995325632 ) ) ;
#3172 = CARTESIAN_POINT ( 'NONE',  ( -30.80549002841696193, 5.431839045955507927, 0.000000000000000000 ) ) ;
#3173 = CARTESIAN_POINT ( 'NONE',  ( 12.67103257592000176, -18.67535491604046172, 6.269892079155907183 ) ) ;
#3174 = CARTESIAN_POINT ( 'NONE',  ( -1.925499516411631973, -10.42380411186744382, 2.516177120048874283 ) ) ;
#3175 = VERTEX_POINT ( 'NONE', #14760 ) ;
#3176 = CARTESIAN_POINT ( 'NONE',  ( -13.37499999999998401, -20.99999999999998934, 2.439580858552613751 ) ) ;
#3177 = CARTESIAN_POINT ( 'NONE',  ( 10.18924542913430820, 10.00000000000000000, 0.000000000000000000 ) ) ;
#3178 = CARTESIAN_POINT ( 'NONE',  ( 7.378441417683177406, -24.50000000000000000, 3.449312527122335048 ) ) ;
#3179 = CARTESIAN_POINT ( 'NONE',  ( -12.52780858231679773, -22.97900456129165647, 3.964901035250747885 ) ) ;
#3180 = ORIENTED_EDGE ( 'NONE', *, *, #17282, .F. ) ;
#3181 = CARTESIAN_POINT ( 'NONE',  ( 13.43273460392801155, -18.08440250163749496, 6.268067769197452677 ) ) ;
#3182 = PLANE ( 'NONE',  #4037 ) ;
#3183 = CARTESIAN_POINT ( 'NONE',  ( -10.49999999999999822, -9.999999999999992895, 1.000000000000000000 ) ) ;
#3184 = ORIENTED_EDGE ( 'NONE', *, *, #1560, .T. ) ;
#3185 = ORIENTED_EDGE ( 'NONE', *, *, #1435, .F. ) ;
#3186 = CARTESIAN_POINT ( 'NONE',  ( 0.000000000000000000, 9.000000000000001776, 1.000000000000000000 ) ) ;
#3187 = AXIS2_PLACEMENT_3D ( 'NONE', #9363, #16628, #4194 ) ;
#3188 = EDGE_CURVE ( 'NONE', #16474, #4026, #16739, .T. ) ;
#3189 = FACE_OUTER_BOUND ( 'NONE', #16253, .T. ) ;
#3190 = VERTEX_POINT ( 'NONE', #13496 ) ;
#3191 = LINE ( 'NONE', #17904, #16020 ) ;
#3192 = VECTOR ( 'NONE', #7285, 1000.000000000000000 ) ;
#3193 = CARTESIAN_POINT ( 'NONE',  ( 14.31494360078803041, 0.000000000000000000, 1.000000000000000000 ) ) ;
#3194 = CARTESIAN_POINT ( 'NONE',  ( 1.619022621591186928, -9.864917468222230923, 1.622643865078341907 ) ) ;
#3195 = DIRECTION ( 'NONE',  ( 1.000000000000000000, 8.673617379884045333E-17, -0.000000000000000000 ) ) ;
#3196 = CARTESIAN_POINT ( 'NONE',  ( 10.49999999999999645, -9.999999999999991118, 1.000000000000000000 ) ) ;
#3197 = PLANE ( 'NONE',  #15035 ) ;
#3198 = CARTESIAN_POINT ( 'NONE',  ( 27.50000000000000355, 3.000000000000000888, 1.000000000000000000 ) ) ;
#3199 = CARTESIAN_POINT ( 'NONE',  ( -11.77780858231679417, -20.27099543870833642, 2.724438792969431589 ) ) ;
#3200 = CARTESIAN_POINT ( 'NONE',  ( -2.583953725994688533, -9.847075946378776479, 2.560676788604062004 ) ) ;
#3201 = VECTOR ( 'NONE', #20273, 1000.000000000000000 ) ;
#3202 = CARTESIAN_POINT ( 'NONE',  ( 6.628441417683177406, -20.99999999999999645, 3.550687472877664952 ) ) ;
#3203 = CARTESIAN_POINT ( 'NONE',  ( -13.12529397353891270, 5.014845663890295846, 3.333333333333220239 ) ) ;
#3204 = CARTESIAN_POINT ( 'NONE',  ( -11.49655858231679417, -22.05068747287764452, 1.749999999999998446 ) ) ;
#3205 = CARTESIAN_POINT ( 'NONE',  ( -6.347191417683176518, -20.91377862118959285, 1.020995438708345082 ) ) ;
#3206 = ORIENTED_EDGE ( 'NONE', *, *, #7111, .F. ) ;
#3207 = CARTESIAN_POINT ( 'NONE',  ( 13.09553549038190567, 4.262042264285192950, 5.042530537310905281 ) ) ;
#3208 = DIRECTION ( 'NONE',  ( -1.000000000000000000, 0.000000000000000000, 0.000000000000000000 ) ) ;
#3209 = VERTEX_POINT ( 'NONE', #16431 ) ;
#3210 = ORIENTED_EDGE ( 'NONE', *, *, #927, .T. ) ;
#3211 = DIRECTION ( 'NONE',  ( 0.000000000000000000, 0.000000000000000000, -1.000000000000000000 ) ) ;
#3212 = EDGE_LOOP ( 'NONE', ( #10514, #13137, #15398, #3641 ) ) ;
#3213 = DIRECTION ( 'NONE',  ( 0.000000000000000000, 0.000000000000000000, 1.000000000000000000 ) ) ;
#3214 = ORIENTED_EDGE ( 'NONE', *, *, #871, .F. ) ;
#3215 = DIRECTION ( 'NONE',  ( -1.000000000000000000, 0.000000000000000000, 0.000000000000000000 ) ) ;
#3216 = EDGE_CURVE ( 'NONE', #9688, #2075, #15171, .T. ) ;
#3217 = CARTESIAN_POINT ( 'NONE',  ( -1.791727654783324741, -9.894249715907907472, 2.380176972254574697 ) ) ;
#3218 = DIRECTION ( 'NONE',  ( -0.000000000000000000, -0.000000000000000000, -1.000000000000000000 ) ) ;
#3219 = CARTESIAN_POINT ( 'NONE',  ( -12.34030858231679240, -22.67418626127525982, 5.270995438708342640 ) ) ;
#3220 = LINE ( 'NONE', #9702, #11950 ) ;
#3221 = ADVANCED_FACE ( 'NONE', ( #7229 ), #11924, .T. ) ;
#3222 = EDGE_CURVE ( 'NONE', #12251, #18418, #3673, .T. ) ;
#3223 = CARTESIAN_POINT ( 'NONE',  ( 7.847191417683175629, -20.91377862118959285, 1.020995438708345082 ) ) ;
#3224 = CARTESIAN_POINT ( 'NONE',  ( -12.34719141768317741, -21.53509896474923835, 2.520995438708346192 ) ) ;
#3225 = ORIENTED_EDGE ( 'NONE', *, *, #5453, .F. ) ;
#3226 = CARTESIAN_POINT ( 'NONE',  ( 5.309058582316794173, -23.27327832286945153, 2.298404588716537411 ) ) ;
#3227 = LINE ( 'NONE', #3326, #16429 ) ;
#3228 = CARTESIAN_POINT ( 'NONE',  ( -12.65816212372154403, -19.32531275206247301, 6.255900543948403225 ) ) ;
#3229 = ORIENTED_EDGE ( 'NONE', *, *, #409, .T. ) ;
#3230 = CARTESIAN_POINT ( 'NONE',  ( 8.590308582316794173, -21.32581373872472597, 1.729004561291657582 ) ) ;
#3231 = DIRECTION ( 'NONE',  ( 0.000000000000000000, -1.000000000000000000, 0.000000000000000000 ) ) ;
#3232 = ORIENTED_EDGE ( 'NONE', *, *, #15898, .T. ) ;
#3233 = LINE ( 'NONE', #11086, #11275 ) ;
#3234 = ORIENTED_EDGE ( 'NONE', *, *, #18519, .T. ) ;
#3235 = CARTESIAN_POINT ( 'NONE',  ( 12.00000000000000178, -18.50000000000000355, 1.000000000000000000 ) ) ;
#3236 = ORIENTED_EDGE ( 'NONE', *, *, #13283, .F. ) ;
#3237 = CARTESIAN_POINT ( 'NONE',  ( -5.121558582316794173, -23.74999999999999645, 3.550687472877651629 ) ) ;
#3238 = CARTESIAN_POINT ( 'NONE',  ( 12.62499999999999289, -20.24999999999899103, 3.700614806296627979 ) ) ;
#3239 = ADVANCED_FACE ( 'NONE', ( #8490 ), #5452, .T. ) ;
#3240 = CARTESIAN_POINT ( 'NONE',  ( -7.369520639128046113, 9.000000000000001776, 0.000000000000000000 ) ) ;
#3241 = CARTESIAN_POINT ( 'NONE',  ( 1.548630333695928618, -9.864917468222230923, 1.622643865078341907 ) ) ;
#3242 = DIRECTION ( 'NONE',  ( 0.000000000000000000, 0.000000000000000000, 1.000000000000000000 ) ) ;
#3243 = CARTESIAN_POINT ( 'NONE',  ( -13.84501469867711698, 4.235742283194553259, 4.666666666666618113 ) ) ;
#3244 = CARTESIAN_POINT ( 'NONE',  ( 6.621558582316794173, -23.74999999999999645, 3.550687472877651629 ) ) ;
#3245 = CARTESIAN_POINT ( 'NONE',  ( -13.90439735423812273, 5.734566389025032684, 4.333333333333380999 ) ) ;
#3246 = DIRECTION ( 'NONE',  ( 1.000000000000000000, 0.000000000000000000, 0.000000000000000000 ) ) ;
#3247 = CARTESIAN_POINT ( 'NONE',  ( -8.121558582316795949, -24.50000000000000000, 3.550687472877651629 ) ) ;
#3248 = CARTESIAN_POINT ( 'NONE',  ( 9.059058582316794173, -20.72672167713054137, 4.701595411283463477 ) ) ;
#3249 = VECTOR ( 'NONE', #10570, 1000.000000000000000 ) ;
#3250 = EDGE_CURVE ( 'NONE', #13, #5953, #534, .T. ) ;
#3251 = CARTESIAN_POINT ( 'NONE',  ( 7.940941417683175629, -21.25705176302044208, 2.828734674606458555 ) ) ;
#3252 = CARTESIAN_POINT ( 'NONE',  ( -9.159691417683177406, -22.67418626127524917, 1.729004561291651587 ) ) ;
#3253 = VERTEX_POINT ( 'NONE', #13592 ) ;
#3254 = CARTESIAN_POINT ( 'NONE',  ( 13.84501469867711698, 4.235742283194553259, 2.999999999999999556 ) ) ;
#3255 = AXIS2_PLACEMENT_3D ( 'NONE', #7664, #969, #1391 ) ;
#3256 = DIRECTION ( 'NONE',  ( 1.000000000000000000, -0.000000000000000000, 0.000000000000000000 ) ) ;
#3257 = ORIENTED_EDGE ( 'NONE', *, *, #7457, .F. ) ;
#3258 = ORIENTED_EDGE ( 'NONE', *, *, #5509, .T. ) ;
#3259 = CARTESIAN_POINT ( 'NONE',  ( -3.997260319564023501, 4.999999999999999112, 0.000000000000000000 ) ) ;
#3260 = DIRECTION ( 'NONE',  ( 0.000000000000000000, 0.000000000000000000, -1.000000000000000000 ) ) ;
#3261 = CYLINDRICAL_SURFACE ( 'NONE', #1910, 1.000000000000002665 ) ;
#3262 = EDGE_CURVE ( 'NONE', #12726, #19461, #13391, .T. ) ;
#3263 = EDGE_CURVE ( 'NONE', #6051, #42, #16842, .T. ) ;
#3264 = CARTESIAN_POINT ( 'NONE',  ( -1.126276606324276619, -9.114917468222230923, 2.372643865078341019 ) ) ;
#3265 = DIRECTION ( 'NONE',  ( 0.000000000000000000, 1.000000000000000000, 0.000000000000000000 ) ) ;
#3266 = DIRECTION ( 'NONE',  ( -0.000000000000000000, -0.000000000000000000, -1.000000000000000000 ) ) ;
#3267 = CARTESIAN_POINT ( 'NONE',  ( -13.11514659413808737, 4.502403003978772134, 5.887634658581065494 ) ) ;
#3268 = CARTESIAN_POINT ( 'NONE',  ( -22.85856191738413656, 9.000000000000001776, 1.000000000000000000 ) ) ;
#3269 = PLANE ( 'NONE',  #17416 ) ;
#3270 = CARTESIAN_POINT ( 'NONE',  ( 13.15498530132288479, 5.764257716805535559, 2.999999999999999556 ) ) ;
#3271 = CARTESIAN_POINT ( 'NONE',  ( -1.665360951492234287, -9.864914341757378580, 1.622643062139706993 ) ) ;
#3272 = ORIENTED_EDGE ( 'NONE', *, *, #339, .F. ) ;
#3273 = CARTESIAN_POINT ( 'NONE',  ( -13.87470602645761986, 4.985154336109792972, 4.791666666666685614 ) ) ;
#3274 = CARTESIAN_POINT ( 'NONE',  ( 0.000000000000000000, 16.00000000000000000, 1.000000000000000000 ) ) ;
#3275 = CARTESIAN_POINT ( 'NONE',  ( 4.659691417683177406, -22.98484643305507191, 0.9790045612916508100 ) ) ;
#3276 = CARTESIAN_POINT ( 'NONE',  ( -4.840308582316795061, -22.36352608949544418, 4.520995438708343528 ) ) ;
#3277 = ORIENTED_EDGE ( 'NONE', *, *, #12484, .T. ) ;
#3278 = CARTESIAN_POINT ( 'NONE',  ( 13.71569110726703045, -3.795099083046435506, 6.575359435862661250 ) ) ;
#3279 = CARTESIAN_POINT ( 'NONE',  ( 13.10624331898488037, 4.052787608736739600, 6.006964772046813117 ) ) ;
#3280 = DIRECTION ( 'NONE',  ( 1.000000000000000000, 0.000000000000000000, -0.000000000000000000 ) ) ;
#3281 = EDGE_LOOP ( 'NONE', ( #3636, #7383, #3386, #18163 ) ) ;
#3282 = EDGE_LOOP ( 'NONE', ( #4373, #558, #13437, #1279 ) ) ;
#3283 = CARTESIAN_POINT ( 'NONE',  ( -15.00000000000000000, 0.000000000000000000, 2.000000000000000000 ) ) ;
#3284 = LINE ( 'NONE', #14255, #2223 ) ;
#3285 = AXIS2_PLACEMENT_3D ( 'NONE', #18381, #18068, #2367 ) ;
#3286 = CARTESIAN_POINT ( 'NONE',  ( 11.00000000000000000, -23.83493649053891517, 5.249999999999999112 ) ) ;
#3287 = CARTESIAN_POINT ( 'NONE',  ( 0.000000000000000000, 10.00000000000000000, 1.000000000000000000 ) ) ;
#3288 = CARTESIAN_POINT ( 'NONE',  ( 2.124709647372160060, -10.68204274815009924, 1.832497960681391147 ) ) ;
#3289 = DIRECTION ( 'NONE',  ( 1.000000000000000000, 0.000000000000000000, -0.000000000000000000 ) ) ;
#3290 = DIRECTION ( 'NONE',  ( 0.000000000000000000, 1.000000000000000000, 0.000000000000000000 ) ) ;
#3291 = DIRECTION ( 'NONE',  ( 0.000000000000000000, 5.204170427930421283E-15, 1.000000000000000000 ) ) ;
#3292 = LINE ( 'NONE', #15943, #17664 ) ;
#3293 = CARTESIAN_POINT ( 'NONE',  ( -12.43405858231679417, -23.20159541128345992, 4.773278322869455970 ) ) ;
#3294 = CARTESIAN_POINT ( 'NONE',  ( -2.203959450683124377, -9.262433282444222371, 2.410528873095051594 ) ) ;
#3295 = AXIS2_PLACEMENT_3D ( 'NONE', #17829, #13417, #14883 ) ;
#3296 = CIRCLE ( 'NONE', #5975, 1.000000000000002665 ) ;
#3297 = CARTESIAN_POINT ( 'NONE',  ( 9.434058582316795949, -22.67126532539354855, 4.242948236979545484 ) ) ;
#3298 = CARTESIAN_POINT ( 'NONE',  ( -13.07121011584135672, 3.033610849983475521, 5.236678440007632496 ) ) ;
#3299 = CARTESIAN_POINT ( 'NONE',  ( -11.68405858231679417, -20.79840458871652942, 2.226721677130544030 ) ) ;
#3300 = ADVANCED_FACE ( 'NONE', ( #18424 ), #2509, .T. ) ;
#3301 = CARTESIAN_POINT ( 'NONE',  ( -12.34719141768317563, -21.22443879296941915, 1.770995438708345748 ) ) ;
#3302 = VECTOR ( 'NONE', #8218, 1000.000000000000000 ) ;
#3303 = ORIENTED_EDGE ( 'NONE', *, *, #12397, .F. ) ;
#3304 = CARTESIAN_POINT ( 'NONE',  ( 13.83770801678722329, 3.866754847752558621, 5.240062463382368030 ) ) ;
#3305 = CARTESIAN_POINT ( 'NONE',  ( 25.04469207716615031, 9.000000000000001776, 1.000000000000000000 ) ) ;
#3306 = ORIENTED_EDGE ( 'NONE', *, *, #19763, .F. ) ;
#3307 = VECTOR ( 'NONE', #19013, 1000.000000000000000 ) ;
#3308 = ORIENTED_EDGE ( 'NONE', *, *, #6444, .T. ) ;
#3309 = DIRECTION ( 'NONE',  ( -0.000000000000000000, -1.000000000000000000, 0.000000000000000000 ) ) ;
#3310 = ORIENTED_EDGE ( 'NONE', *, *, #7828, .T. ) ;
#3311 = DIRECTION ( 'NONE',  ( 0.000000000000000000, 0.000000000000000000, -1.000000000000000000 ) ) ;
#3312 = CIRCLE ( 'NONE', #4652, 1.000000000000002665 ) ;
#3313 = ORIENTED_EDGE ( 'NONE', *, *, #19126, .T. ) ;
#3314 = CARTESIAN_POINT ( 'NONE',  ( 10.28469141768317741, -23.77099543870834353, 4.174186261275251830 ) ) ;
#3315 = DIRECTION ( 'NONE',  ( -1.000000000000000000, 0.000000000000000000, 0.000000000000000000 ) ) ;
#3316 = VECTOR ( 'NONE', #16099, 1000.000000000000000 ) ;
#3317 = CARTESIAN_POINT ( 'NONE',  ( -1.126276606324276619, -9.114917468222230923, 2.372643865078341019 ) ) ;
#3318 = CARTESIAN_POINT ( 'NONE',  ( 2.616536356806028696, -10.07836329504444706, 2.620076000170431296 ) ) ;
#3319 = CARTESIAN_POINT ( 'NONE',  ( -13.09030858231679417, -21.32581373872472952, 1.729004561291657138 ) ) ;
#3320 = DIRECTION ( 'NONE',  ( 1.000000000000000000, 0.000000000000000000, 0.000000000000000000 ) ) ;
#3321 = CARTESIAN_POINT ( 'NONE',  ( 7.003441417683177406, -22.05068747287765873, 5.250000000000000888 ) ) ;
#3322 = PLANE ( 'NONE',  #2192 ) ;
#3323 = CARTESIAN_POINT ( 'NONE',  ( -11.03469141768317741, -20.97900456129164581, 3.136473910504570917 ) ) ;
#3324 = ORIENTED_EDGE ( 'NONE', *, *, #20088, .T. ) ;
#3325 = CARTESIAN_POINT ( 'NONE',  ( 7.934058582316796837, -23.73192549717337130, 5.303608408759367343 ) ) ;
#3326 = CARTESIAN_POINT ( 'NONE',  ( 7.619520639128047002, 0.000000000000000000, 1.000000000000000000 ) ) ;
#3327 = CARTESIAN_POINT ( 'NONE',  ( -12.62543384439201510, -20.97809085820452424, 4.782403934559678937 ) ) ;
#3328 = ORIENTED_EDGE ( 'NONE', *, *, #13242, .F. ) ;
#3329 = ADVANCED_FACE ( 'NONE', ( #5345 ), #2412, .T. ) ;
#3330 = CARTESIAN_POINT ( 'NONE',  ( 5.684058582316794173, -20.79840458871652942, 2.226721677130544030 ) ) ;
#3331 = CARTESIAN_POINT ( 'NONE',  ( -22.81633994409548549, 10.00000000000000000, 1.000000000000000000 ) ) ;
#3332 = CIRCLE ( 'NONE', #11346, 2.500000000000000444 ) ;
#3333 = ORIENTED_EDGE ( 'NONE', *, *, #2896, .T. ) ;
#3334 = LINE ( 'NONE', #6379, #252 ) ;
#3335 = PRODUCT_CONTEXT ( 'NONE', #6262, 'mechanical' ) ;
#3336 = ORIENTED_EDGE ( 'NONE', *, *, #17550, .T. ) ;
#3337 = AXIS2_PLACEMENT_3D ( 'NONE', #15356, #16825, #2489 ) ;
#3338 = DIRECTION ( 'NONE',  ( 1.000000000000000000, 0.000000000000000000, 0.000000000000000000 ) ) ;
#3339 = EDGE_CURVE ( 'NONE', #15255, #4739, #8901, .T. ) ;
#3340 = EDGE_CURVE ( 'NONE', #8718, #13902, #12029, .T. ) ;
#3341 = ORIENTED_EDGE ( 'NONE', *, *, #15117, .T. ) ;
#3342 = CARTESIAN_POINT ( 'NONE',  ( -5.215308582316793284, -23.77099543870833998, 2.825813738724734847 ) ) ;
#3343 = CARTESIAN_POINT ( 'NONE',  ( 12.62672070884157804, -20.24999999999983658, 3.550922209436377042 ) ) ;
#3344 = AXIS2_PLACEMENT_3D ( 'NONE', #1495, #20449, #14143 ) ;
#3345 = CARTESIAN_POINT ( 'NONE',  ( 26.79469207716614676, 9.000000000000001776, 0.000000000000000000 ) ) ;
#3346 = CARTESIAN_POINT ( 'NONE',  ( 0.9854920305337621089, -9.114917468222230923, 1.622643865078341463 ) ) ;
#3347 = CARTESIAN_POINT ( 'NONE',  ( 12.64751377014909828, -19.11305460747000495, 5.510446717915143289 ) ) ;
#3348 = CARTESIAN_POINT ( 'NONE',  ( -0.000000000000000000, 11.64110105645932691, 0.000000000000000000 ) ) ;
#3349 = CARTESIAN_POINT ( 'NONE',  ( -13.82092246150448211, 3.019084305971233562, 5.221833296715730377 ) ) ;
#3350 = CARTESIAN_POINT ( 'NONE',  ( 11.49655858231679595, -22.05068747287764452, 0.9999999999999978906 ) ) ;
#3351 = CARTESIAN_POINT ( 'NONE',  ( -13.90439735423812273, 5.734566389025032684, 2.999999999999999556 ) ) ;
#3352 = VECTOR ( 'NONE', #8217, 1000.000000000000000 ) ;
#3353 = CARTESIAN_POINT ( 'NONE',  ( 0.000000000000000000, 9.000000000000001776, 1.000000000000000000 ) ) ;
#3354 = CARTESIAN_POINT ( 'NONE',  ( 6.434058582316794173, -23.20159541128345992, 4.773278322869455970 ) ) ;
#3355 = EDGE_CURVE ( 'NONE', #17557, #5957, #7333, .T. ) ;
#3356 = CARTESIAN_POINT ( 'NONE',  ( 7.190941417683177406, -22.74294823697955081, 4.171265325393542334 ) ) ;
#3357 = CARTESIAN_POINT ( 'NONE',  ( -8.409691417683177406, -21.32581373872474373, 5.270995438708348857 ) ) ;
#3358 = ORIENTED_EDGE ( 'NONE', *, *, #6057, .F. ) ;
#3359 = VERTEX_POINT ( 'NONE', #635 ) ;
#3360 = CARTESIAN_POINT ( 'NONE',  ( 13.84485691484488257, 4.227774199669918964, 5.063753864839139140 ) ) ;
#3361 = FACE_OUTER_BOUND ( 'NONE', #8272, .T. ) ;
#3362 = ORIENTED_EDGE ( 'NONE', *, *, #6706, .T. ) ;
#3363 = EDGE_LOOP ( 'NONE', ( #17972, #9302, #11307, #5959 ) ) ;
#3364 = DIRECTION ( 'NONE',  ( 0.000000000000000000, -0.2588190451025247363, -0.9659258262890673130 ) ) ;
#3365 = ADVANCED_FACE ( 'NONE', ( #20103 ), #5766, .T. ) ;
#3366 = EDGE_CURVE ( 'NONE', #9600, #2799, #8587, .T. ) ;
#3367 = FACE_OUTER_BOUND ( 'NONE', #331, .T. ) ;
#3368 = VECTOR ( 'NONE', #18881, 1000.000000000000000 ) ;
#3369 = VECTOR ( 'NONE', #5055, 1000.000000000000000 ) ;
#3370 = CARTESIAN_POINT ( 'NONE',  ( -13.12424783836753228, 4.962015837561366993, 5.328858059679200565 ) ) ;
#3371 = CARTESIAN_POINT ( 'NONE',  ( -3.451187703687236041, -10.75258211228477734, 2.985843844067104680 ) ) ;
#3372 = PLANE ( 'NONE',  #18036 ) ;
#3373 = DIRECTION ( 'NONE',  ( -1.000000000000000000, 0.000000000000000000, 0.000000000000000000 ) ) ;
#3374 = CARTESIAN_POINT ( 'NONE',  ( -12.64131715375063258, -19.42598373559290792, 5.491151580003103660 ) ) ;
#3375 = CARTESIAN_POINT ( 'NONE',  ( 12.05905858231679417, -20.72672167713054137, 4.701595411283463477 ) ) ;
#3376 = CARTESIAN_POINT ( 'NONE',  ( 21.67243175760212637, 4.999999999999999112, 1.000000000000000000 ) ) ;
#3377 = CARTESIAN_POINT ( 'NONE',  ( 12.69740987707854707, -17.34330120752609616, 6.298537912489285517 ) ) ;
#3378 = CARTESIAN_POINT ( 'NONE',  ( -2.022757268986824730, -10.07035769906783784, 1.675405020440470238 ) ) ;
#3379 = ORIENTED_EDGE ( 'NONE', *, *, #14251, .F. ) ;
#3380 = CARTESIAN_POINT ( 'NONE',  ( -13.85403523778986390, 3.941279508358651817, 5.991705257707216958 ) ) ;
#3381 = DIRECTION ( 'NONE',  ( 1.000000000000000000, 0.000000000000000000, 0.000000000000000000 ) ) ;
#3382 = VECTOR ( 'NONE', #16870, 1000.000000000000000 ) ;
#3383 = EDGE_CURVE ( 'NONE', #2461, #20415, #7025, .T. ) ;
#3384 = CARTESIAN_POINT ( 'NONE',  ( 3.974842109207560537, -21.73478823434188456, 6.006404853634143670 ) ) ;
#3385 = CARTESIAN_POINT ( 'NONE',  ( -8.027808582316795949, -22.97900456129165647, 3.964901035250747885 ) ) ;
#3386 = ORIENTED_EDGE ( 'NONE', *, *, #7138, .F. ) ;
#3387 = CIRCLE ( 'NONE', #19421, 2.500000000000000444 ) ;
#3388 = CARTESIAN_POINT ( 'NONE',  ( 13.83079205777725917, 2.017498917744843023, 6.700359435863729729 ) ) ;
#3389 = CARTESIAN_POINT ( 'NONE',  ( 13.10192273101908000, 3.834597916462216816, 6.003936301248457674 ) ) ;
#3390 = DIRECTION ( 'NONE',  ( 8.673617379884033500E-16, -1.000000000000000000, 0.000000000000000000 ) ) ;
#3391 = EDGE_LOOP ( 'NONE', ( #15808, #5113, #10155, #11308 ) ) ;
#3392 = VERTEX_POINT ( 'NONE', #8693 ) ;
#3393 = LINE ( 'NONE', #3186, #7762 ) ;
#3394 = CARTESIAN_POINT ( 'NONE',  ( 6.063547257480584207, 10.00000000000000000, 0.000000000000000000 ) ) ;
#3395 = VERTEX_POINT ( 'NONE', #15064 ) ;
#3396 = CIRCLE ( 'NONE', #73, 10.00000000000000000 ) ;
#3397 = FACE_OUTER_BOUND ( 'NONE', #13302, .T. ) ;
#3398 = CARTESIAN_POINT ( 'NONE',  ( 2.110348196723525138, -10.58007678474401914, 1.806311064303893099 ) ) ;
#3399 = FACE_OUTER_BOUND ( 'NONE', #19377, .T. ) ;
#3400 = CARTESIAN_POINT ( 'NONE',  ( -4.250698171653726654, 11.64110105645932691, 0.000000000000000000 ) ) ;
#3401 = CARTESIAN_POINT ( 'NONE',  ( -10.49999999999999822, -9.999999999999992895, 2.000000000000000000 ) ) ;
#3402 = CARTESIAN_POINT ( 'NONE',  ( -5.563547257480587760, 10.00000000000000000, 1.000000000000000000 ) ) ;
#3403 = CARTESIAN_POINT ( 'NONE',  ( -11.87155858231679417, -20.24999999999999289, 3.449312527122348371 ) ) ;
#3404 = CARTESIAN_POINT ( 'NONE',  ( -0.9854920305337621089, -9.114917468222230923, 2.372643865078341019 ) ) ;
#3405 = CARTESIAN_POINT ( 'NONE',  ( -13.09300823383486900, 4.134415808666423331, 5.226944302881396887 ) ) ;
#3406 = CARTESIAN_POINT ( 'NONE',  ( -11.59030858231679417, -21.32581373872472597, 1.729004561291657582 ) ) ;
#3407 = EDGE_CURVE ( 'NONE', #19990, #7441, #12504, .T. ) ;
#3408 = CARTESIAN_POINT ( 'NONE',  ( -6.534691417683176518, -20.22900456129164581, 2.825813738724747726 ) ) ;
#3409 = ORIENTED_EDGE ( 'NONE', *, *, #6382, .F. ) ;
#3410 = EDGE_CURVE ( 'NONE', #17844, #2654, #680, .T. ) ;
#3411 = CARTESIAN_POINT ( 'NONE',  ( 13.38929389708972195, -18.77815819697223887, 4.753083296715700179 ) ) ;
#3412 = CARTESIAN_POINT ( 'NONE',  ( -10.49999999999999822, -9.999999999999992895, 2.500000000000000000 ) ) ;
#3413 = ORIENTED_EDGE ( 'NONE', *, *, #6925, .T. ) ;
#3414 = ORIENTED_EDGE ( 'NONE', *, *, #10183, .T. ) ;
#3415 = VECTOR ( 'NONE', #6864, 1000.000000000000000 ) ;
#3416 = CARTESIAN_POINT ( 'NONE',  ( -3.499999999999997780, -19.49999999999999645, 4.000000000000000000 ) ) ;
#3417 = VERTEX_POINT ( 'NONE', #15637 ) ;
#3418 = DIRECTION ( 'NONE',  ( 0.000000000000000000, 1.000000000000000000, 0.000000000000000000 ) ) ;
#3419 = VECTOR ( 'NONE', #4939, 1000.000000000000000 ) ;
#3420 = ORIENTED_EDGE ( 'NONE', *, *, #720, .T. ) ;
#3421 = VECTOR ( 'NONE', #18309, 1000.000000000000000 ) ;
#3422 = CARTESIAN_POINT ( 'NONE',  ( -2.693754455098655409, -10.04853567022903782, 2.237415670251142519 ) ) ;
#3423 = ADVANCED_FACE ( 'NONE', ( #2889 ), #1124, .F. ) ;
#3424 = PLANE ( 'NONE',  #8675 ) ;
#3425 = CARTESIAN_POINT ( 'NONE',  ( -1.742625132518061504, -9.872369070458363538, 2.374557585393312298 ) ) ;
#3426 = CARTESIAN_POINT ( 'NONE',  ( 2.559937518207947793, -9.746075135043517079, 2.534737762559237773 ) ) ;
#3427 = CARTESIAN_POINT ( 'NONE',  ( -12.80905858231679417, -23.27327832286945153, 2.298404588716537411 ) ) ;
#3428 = VECTOR ( 'NONE', #20442, 1000.000000000000000 ) ;
#3429 = CARTESIAN_POINT ( 'NONE',  ( 27.44203811574919882, 11.64110105645932691, 0.000000000000000000 ) ) ;
#3430 = CARTESIAN_POINT ( 'NONE',  ( 7.284691417683176518, -23.77099543870834353, 4.174186261275252718 ) ) ;
#3431 = DIRECTION ( 'NONE',  ( 1.000000000000000000, 0.000000000000000000, -0.000000000000000000 ) ) ;
#3432 = CARTESIAN_POINT ( 'NONE',  ( -4.847191417683178294, -21.22443879296941915, 1.770995438708345748 ) ) ;
#3433 = ORIENTED_EDGE ( 'NONE', *, *, #14900, .T. ) ;
#3434 = CARTESIAN_POINT ( 'NONE',  ( 9.152808582316795949, -20.91377862118960351, 5.979004561291660913 ) ) ;
#3435 = CARTESIAN_POINT ( 'NONE',  ( 12.64195242771744709, -19.39390240027112000, 5.496549442168085164 ) ) ;
#3436 = CARTESIAN_POINT ( 'NONE',  ( -13.15498566372047762, 5.764276017890828108, 4.942557026581394730 ) ) ;
#3437 = VERTEX_POINT ( 'NONE', #1326 ) ;
#3438 = CYLINDRICAL_SURFACE ( 'NONE', #8619, 10.00000000000000000 ) ;
#3439 = CARTESIAN_POINT ( 'NONE',  ( 2.499999999999999112, -24.49999999999999289, 1.000000000000000000 ) ) ;
#3440 = ORIENTED_EDGE ( 'NONE', *, *, #18783, .F. ) ;
#3441 = VERTEX_POINT ( 'NONE', #17211 ) ;
#3442 = VECTOR ( 'NONE', #3468, 1000.000000000000000 ) ;
#3443 = CARTESIAN_POINT ( 'NONE',  ( 12.73791931723291881, -19.98176637867805283, 3.535752669880253940 ) ) ;
#3444 = VERTEX_POINT ( 'NONE', #13863 ) ;
#3445 = CARTESIAN_POINT ( 'NONE',  ( -7.465308582316795061, -20.22900456129164937, 4.174186261275266929 ) ) ;
#3446 = EDGE_CURVE ( 'NONE', #13746, #19940, #20264, .T. ) ;
#3447 = CARTESIAN_POINT ( 'NONE',  ( 12.64931222250080545, -19.02223276370786209, 5.512399842915133519 ) ) ;
#3448 = PLANE ( 'NONE',  #14464 ) ;
#3449 = ADVANCED_FACE ( 'NONE', ( #18901 ), #4559, .T. ) ;
#3450 = CARTESIAN_POINT ( 'NONE',  ( 12.62599079447150885, -20.19996487918709249, 4.820256282269618886 ) ) ;
#3451 = LINE ( 'NONE', #3861, #20059 ) ;
#3452 = CARTESIAN_POINT ( 'NONE',  ( -13.37499999999998579, -20.24999999999999289, 3.666666666666653640 ) ) ;
#3453 = CARTESIAN_POINT ( 'NONE',  ( 11.68405858231679595, -20.26807450282662160, 1.696391591240633101 ) ) ;
#3454 = CARTESIAN_POINT ( 'NONE',  ( -13.15452713448031297, 5.741120291255121799, 5.290164123766007087 ) ) ;
#3455 = CARTESIAN_POINT ( 'NONE',  ( -11.22219141768317741, -19.52099543870834353, 4.586221378810406257 ) ) ;
#3456 = LINE ( 'NONE', #14636, #18079 ) ;
#3457 = CARTESIAN_POINT ( 'NONE',  ( -0.000000000000000000, 10.00000000000000000, 0.000000000000000000 ) ) ;
#3458 = CARTESIAN_POINT ( 'NONE',  ( 12.43405858231679595, -22.67126532539354855, 4.242948236979545484 ) ) ;
#3459 = CARTESIAN_POINT ( 'NONE',  ( -8.034691417683175629, -20.22900456129164581, 2.825813738724748170 ) ) ;
#3460 = ORIENTED_EDGE ( 'NONE', *, *, #13953, .T. ) ;
#3461 = ORIENTED_EDGE ( 'NONE', *, *, #13218, .T. ) ;
#3462 = CARTESIAN_POINT ( 'NONE',  ( 13.84090061271218985, 4.027980941966571748, 5.240332426532912535 ) ) ;
#3463 = PLANE ( 'NONE',  #9769 ) ;
#3464 = CARTESIAN_POINT ( 'NONE',  ( 15.36404127825609400, 4.999999999999999112, 0.000000000000000000 ) ) ;
#3465 = EDGE_LOOP ( 'NONE', ( #16160, #5425, #10306, #917, #71, #16273, #4474, #10670 ) ) ;
#3466 = AXIS2_PLACEMENT_3D ( 'NONE', #6909, #10154, #16525 ) ;
#3467 = ORIENTED_EDGE ( 'NONE', *, *, #8721, .F. ) ;
#3468 = DIRECTION ( 'NONE',  ( 0.000000000000000000, 1.000000000000000000, -0.000000000000000000 ) ) ;
#3469 = CARTESIAN_POINT ( 'NONE',  ( -24.50000000000000000, 3.000000000000000888, 0.000000000000000000 ) ) ;
#3470 = CARTESIAN_POINT ( 'NONE',  ( -13.12529397354238192, 5.014845663890295846, 4.916666666666650087 ) ) ;
#3471 = FACE_BOUND ( 'NONE', #1995, .T. ) ;
#3472 = EDGE_CURVE ( 'NONE', #17017, #9770, #10530, .T. ) ;
#3473 = LINE ( 'NONE', #17905, #14731 ) ;
#3474 = AXIS2_PLACEMENT_3D ( 'NONE', #2760, #978, #9138 ) ;
#3475 = CARTESIAN_POINT ( 'NONE',  ( -13.12503131243110843, 5.001581277770153378, 5.166347330538456184 ) ) ;
#3476 = CARTESIAN_POINT ( 'NONE',  ( 7.652808582316794173, -21.22443879296942626, 5.229004561291660025 ) ) ;
#3477 = DIRECTION ( 'NONE',  ( 1.000000000000000000, 0.000000000000000000, 0.000000000000000000 ) ) ;
#3478 = CARTESIAN_POINT ( 'NONE',  ( 13.09293046926041626, 3.380488697651010011, 5.994170676248444352 ) ) ;
#3479 = CARTESIAN_POINT ( 'NONE',  ( 0.000000000000000000, 11.64110105645932691, 10.00000000000000000 ) ) ;
#3480 = ADVANCED_FACE ( 'NONE', ( #10943 ), #4357, .T. ) ;
#3481 = ORIENTED_EDGE ( 'NONE', *, *, #4137, .T. ) ;
#3482 = EDGE_CURVE ( 'NONE', #1664, #11612, #15539, .T. ) ;
#3483 = CARTESIAN_POINT ( 'NONE',  ( -13.43259567872942917, -17.34141822415733714, 5.534013032956523581 ) ) ;
#3484 = LINE ( 'NONE', #9762, #12382 ) ;
#3485 = CARTESIAN_POINT ( 'NONE',  ( 5.503441417683177406, -22.05068747287766229, 6.000000000000001776 ) ) ;
#3486 = CARTESIAN_POINT ( 'NONE',  ( -5.965308582316795949, -20.97900456129165647, 3.863526089495444626 ) ) ;
#3487 = ORIENTED_EDGE ( 'NONE', *, *, #1116, .T. ) ;
#3488 = CARTESIAN_POINT ( 'NONE',  ( 12.62499999998404299, -20.99999999996810729, 2.793053905886972998 ) ) ;
#3489 = CARTESIAN_POINT ( 'NONE',  ( 13.10821839766814279, 4.152529082241303904, 5.997503362667785609 ) ) ;
#3490 = CARTESIAN_POINT ( 'NONE',  ( -13.37499999884080637, -20.15165736766552484, 3.448843054164315802 ) ) ;
#3491 = ORIENTED_EDGE ( 'NONE', *, *, #2402, .F. ) ;
#3492 = ORIENTED_EDGE ( 'NONE', *, *, #7758, .T. ) ;
#3493 = DIRECTION ( 'NONE',  ( 0.000000000000000000, 1.000000000000000000, -0.000000000000000000 ) ) ;
#3494 = CARTESIAN_POINT ( 'NONE',  ( 14.50000000000001243, -25.49999999999999645, 4.000000000000000000 ) ) ;
#3495 = LINE ( 'NONE', #9974, #10646 ) ;
#3496 = EDGE_CURVE ( 'NONE', #16502, #9634, #23, .T. ) ;
#3497 = LINE ( 'NONE', #9875, #11009 ) ;
#3498 = CARTESIAN_POINT ( 'NONE',  ( 1.733187991654075777, -9.867296153774269385, 1.623254759047128237 ) ) ;
#3499 = LINE ( 'NONE', #1927, #12059 ) ;
#3500 = CARTESIAN_POINT ( 'NONE',  ( 3.747260319564023501, 9.000000000000001776, 0.000000000000000000 ) ) ;
#3501 = CARTESIAN_POINT ( 'NONE',  ( -14.49999999999998579, -19.49999999999999645, 1.000000000000000000 ) ) ;
#3502 = CARTESIAN_POINT ( 'NONE',  ( 0.000000000000000000, 4.999999999999999112, 1.000000000000000000 ) ) ;
#3503 = CARTESIAN_POINT ( 'NONE',  ( 13.00000000000000355, 7.806255641895631925E-15, 1.000000000000000000 ) ) ;
#3504 = CARTESIAN_POINT ( 'NONE',  ( -3.475298211275419380, -9.785109117490691233, 1.987377451789144933 ) ) ;
#3505 = ORIENTED_EDGE ( 'NONE', *, *, #1195, .T. ) ;
#3506 = CARTESIAN_POINT ( 'NONE',  ( -13.09494140422671471, 4.232040913449062636, 5.131376921800749003 ) ) ;
#3507 = CARTESIAN_POINT ( 'NONE',  ( -5.121558582316795061, -22.99999999999999645, 3.550687472877652073 ) ) ;
#3508 = CARTESIAN_POINT ( 'NONE',  ( -9.159691417683179182, -22.67418626127524917, 1.729004561291651809 ) ) ;
#3509 = ORIENTED_EDGE ( 'NONE', *, *, #5846, .T. ) ;
#3510 = CARTESIAN_POINT ( 'NONE',  ( 13.84497512400090891, 4.233743762047977199, 5.032110966142367303 ) ) ;
#3512 = DIRECTION ( 'NONE',  ( 1.000000000000000000, 0.000000000000000000, 0.000000000000000000 ) ) ;
#3511 = AXIS2_PLACEMENT_3D ( 'NONE', #2208, #15069, #8590 ) ;
#3513 = ORIENTED_EDGE ( 'NONE', *, *, #11312, .T. ) ;
#3514 = CIRCLE ( 'NONE', #20607, 0.4999999999999987232 ) ;
#3515 = ADVANCED_FACE ( 'NONE', ( #13762 ), #9371, .T. ) ;
#3516 = ORIENTED_EDGE ( 'NONE', *, *, #8231, .T. ) ;
#3517 = DIRECTION ( 'NONE',  ( 1.000000000000000000, 0.000000000000000000, -0.000000000000000000 ) ) ;
#3518 = UNCERTAINTY_MEASURE_WITH_UNIT (LENGTH_MEASURE( 1.000000000000000082E-05 ), #13277, 'distance_accuracy_value', 'NONE');
#3519 = ORIENTED_EDGE ( 'NONE', *, *, #14510, .T. ) ;
#3520 = DIRECTION ( 'NONE',  ( -0.000000000000000000, -0.000000000000000000, -1.000000000000000000 ) ) ;
#3521 = EDGE_LOOP ( 'NONE', ( #18263, #4190, #8551, #9985 ) ) ;
#3522 = CARTESIAN_POINT ( 'NONE',  ( 6.347191417683176518, -21.22443879296941915, 1.770995438708345748 ) ) ;
#3523 = CARTESIAN_POINT ( 'NONE',  ( 0.6250000000000005551, 0.000000000000000000, 0.000000000000000000 ) ) ;
#3524 = EDGE_CURVE ( 'NONE', #9059, #4330, #17005, .T. ) ;
#3525 = EDGE_CURVE ( 'NONE', #2170, #15304, #1427, .T. ) ;
#3526 = CARTESIAN_POINT ( 'NONE',  ( -2.567175533087980188, -9.771398394011347577, 2.541241281345096859 ) ) ;
#3527 = CARTESIAN_POINT ( 'NONE',  ( -22.06633994409548194, 10.00000000000000000, 1.000000000000000000 ) ) ;
#3528 = CARTESIAN_POINT ( 'NONE',  ( 0.000000000000000000, 16.00000000000000000, 1.000000000000000000 ) ) ;
#3529 = EDGE_CURVE ( 'NONE', #1441, #3058, #6135, .T. ) ;
#3530 = LINE ( 'NONE', #3123, #3940 ) ;
#3531 = CARTESIAN_POINT ( 'NONE',  ( 11.78469141768317563, -23.77099543870834353, 4.174186261275252718 ) ) ;
#3532 = CARTESIAN_POINT ( 'NONE',  ( 11.00000000000000000, -20.16506350946107418, 5.250000000000000000 ) ) ;
#3533 = CARTESIAN_POINT ( 'NONE',  ( -4.284691417683176518, -23.77099543870834353, 4.174186261275252718 ) ) ;
#3534 = ORIENTED_EDGE ( 'NONE', *, *, #17568, .F. ) ;
#3535 = CARTESIAN_POINT ( 'NONE',  ( 12.90280858231679595, -23.08622137881038938, 1.020995438708339309 ) ) ;
#3536 = CARTESIAN_POINT ( 'NONE',  ( 12.69247507894198712, -16.84250851341299082, 5.559274842915185033 ) ) ;
#3537 = CARTESIAN_POINT ( 'NONE',  ( -12.63465172146706728, -19.76258806590802664, 5.372658420469845986 ) ) ;
#3538 = ORIENTED_EDGE ( 'NONE', *, *, #2203, .T. ) ;
#3539 = CARTESIAN_POINT ( 'NONE',  ( 7.500000000000002665, -9.999999999999991118, 2.500000000000000000 ) ) ;
#3540 = CARTESIAN_POINT ( 'NONE',  ( 2.311130159782011972, 9.000000000000001776, 1.000000000000000000 ) ) ;
#3541 = ORIENTED_EDGE ( 'NONE', *, *, #10425, .T. ) ;
#3542 = AXIS2_PLACEMENT_3D ( 'NONE', #2372, #2471, #7290 ) ;
#3543 = ORIENTED_EDGE ( 'NONE', *, *, #10836, .T. ) ;
#3544 = PLANE ( 'NONE',  #1122 ) ;
#3545 = ORIENTED_EDGE ( 'NONE', *, *, #15013, .F. ) ;
#3546 = CARTESIAN_POINT ( 'NONE',  ( -7.934058582316792396, -23.20159541128345992, 4.773278322869455970 ) ) ;
#3547 = CARTESIAN_POINT ( 'NONE',  ( 14.50000000000000000, -23.00000000000001421, 4.000000000000000000 ) ) ;
#3548 = DIRECTION ( 'NONE',  ( 1.000000000000000000, 2.312964634635756072E-15, 0.000000000000000000 ) ) ;
#3549 = CARTESIAN_POINT ( 'NONE',  ( 12.65051119073526564, -18.96168486786632457, 5.513701926248478102 ) ) ;
#3550 = LINE ( 'NONE', #618, #5335 ) ;
#3551 = CARTESIAN_POINT ( 'NONE',  ( -13.37741471237955260, -20.12805702483293757, 4.993653275319895890 ) ) ;
#3552 = CARTESIAN_POINT ( 'NONE',  ( 9.621558582316795949, -24.50000000000000000, 3.550687472877651629 ) ) ;
#3553 = CARTESIAN_POINT ( 'NONE',  ( -12.62500000000001954, -20.25000000000274269, 4.083333333315724012 ) ) ;
#3554 = CARTESIAN_POINT ( 'NONE',  ( -7.465308582316796837, -19.47900456129164937, 4.484846433055089676 ) ) ;
#3555 = FACE_OUTER_BOUND ( 'NONE', #4637, .T. ) ;
#3556 = PLANE ( 'NONE',  #8080 ) ;
#3557 = EDGE_CURVE ( 'NONE', #5157, #2020, #9068, .T. ) ;
#3558 = CARTESIAN_POINT ( 'NONE',  ( 7.840308582316795949, -22.36352608949544418, 4.520995438708343528 ) ) ;
#3559 = CARTESIAN_POINT ( 'NONE',  ( -5.128441417683177406, -20.24999999999999289, 3.550687472877664952 ) ) ;
#3560 = ORIENTED_EDGE ( 'NONE', *, *, #6746, .T. ) ;
#3561 = ORIENTED_EDGE ( 'NONE', *, *, #16527, .F. ) ;
#3562 = CARTESIAN_POINT ( 'NONE',  ( 13.81612658856640863, 2.776892722604777930, 5.216624963382545666 ) ) ;
#3563 = FACE_OUTER_BOUND ( 'NONE', #9994, .T. ) ;
#3564 = SURFACE_STYLE_FILL_AREA ( #17897 ) ;
#3565 = ORIENTED_EDGE ( 'NONE', *, *, #9382, .F. ) ;
#3566 = CARTESIAN_POINT ( 'NONE',  ( -14.49999999999998401, -25.49999999999999645, 1.000000000000000000 ) ) ;
#3567 = VECTOR ( 'NONE', #1725, 1000.000000000000000 ) ;
#3568 = DIRECTION ( 'NONE',  ( -0.000000000000000000, 0.000000000000000000, -1.000000000000000000 ) ) ;
#3569 = CARTESIAN_POINT ( 'NONE',  ( 13.83065313257865370, 2.760483195222930952, 5.966304699623404595 ) ) ;
#3570 = DIRECTION ( 'NONE',  ( -0.000000000000000000, -0.000000000000000000, -1.000000000000000000 ) ) ;
#3571 = DIRECTION ( 'NONE',  ( -0.000000000000000000, -0.000000000000000000, -1.000000000000000000 ) ) ;
#3572 = CARTESIAN_POINT ( 'NONE',  ( 19.23630159782011617, 9.000000000000001776, 0.000000000000000000 ) ) ;
#3573 = CARTESIAN_POINT ( 'NONE',  ( -12.95145221759166354, -3.764163011652346569, 5.840524842913703552 ) ) ;
#3574 = CARTESIAN_POINT ( 'NONE',  ( 5.215308582316794173, -23.77099543870833998, 2.825813738724734847 ) ) ;
#3575 = CARTESIAN_POINT ( 'NONE',  ( 27.00000000000000000, 0.000000000000000000, 1.000000000000000000 ) ) ;
#3576 = CARTESIAN_POINT ( 'NONE',  ( 13.10431844137356627, 3.955581289335645234, 6.006545679920360925 ) ) ;
#3577 = LINE ( 'NONE', #3793, #6356 ) ;
#3578 = CARTESIAN_POINT ( 'NONE',  ( -13.66279757975024722, -5.716222222589476765, 5.784013032957989964 ) ) ;
#3579 = CARTESIAN_POINT ( 'NONE',  ( 0.000000000000000000, 9.000000000000001776, 1.000000000000000000 ) ) ;
#3580 = CARTESIAN_POINT ( 'NONE',  ( 8.972191417683177406, -23.72900456129165292, 2.724438792969417822 ) ) ;
#3581 = CARTESIAN_POINT ( 'NONE',  ( -8.871558582316795949, -20.99999999999999645, 3.449312527122348371 ) ) ;
#3582 = ORIENTED_EDGE ( 'NONE', *, *, #15346, .F. ) ;
#3583 = CARTESIAN_POINT ( 'NONE',  ( 12.62499999999998224, -20.99999999999998934, 4.291666666666699825 ) ) ;
#3584 = CARTESIAN_POINT ( 'NONE',  ( 13.12529397354238192, 5.014845663890295846, 4.166666666666765551 ) ) ;
#3585 = AXIS2_PLACEMENT_3D ( 'NONE', #412, #16710, #7206 ) ;
#3586 = DIRECTION ( 'NONE',  ( -1.000000000000000000, 0.000000000000000000, 0.000000000000000000 ) ) ;
#3587 = ORIENTED_EDGE ( 'NONE', *, *, #4669, .T. ) ;
#3588 = ADVANCED_FACE ( 'NONE', ( #7808 ), #14170, .T. ) ;
#3589 = ORIENTED_EDGE ( 'NONE', *, *, #553, .F. ) ;
#3590 = LINE ( 'NONE', #7049, #4430 ) ;
#3591 = LINE ( 'NONE', #2436, #1235 ) ;
#3593 = EDGE_CURVE ( 'NONE', #19731, #19600, #15440, .T. ) ;
#3592 = VECTOR ( 'NONE', #2702, 1000.000000000000000 ) ;
#3594 = DIRECTION ( 'NONE',  ( 0.000000000000000000, 1.000000000000000000, -1.304178812473495102E-15 ) ) ;
#3595 = CARTESIAN_POINT ( 'NONE',  ( -25.29469207716615031, 4.999999999999999112, 0.000000000000000000 ) ) ;
#3596 = CARTESIAN_POINT ( 'NONE',  ( 1.963707630584672570, -9.980492102769451535, 1.652325740065381909 ) ) ;
#3597 = DIRECTION ( 'NONE',  ( 1.000000000000000000, 0.000000000000000000, 0.000000000000000000 ) ) ;
#3598 = DIRECTION ( 'NONE',  ( 0.000000000000000000, -0.000000000000000000, 1.000000000000000000 ) ) ;
#3599 = CIRCLE ( 'NONE', #16625, 1.499999999999996225 ) ;
#3600 = CARTESIAN_POINT ( 'NONE',  ( 12.63267999405561071, -20.34063974247287376, 3.549900554235012162 ) ) ;
#3601 = FACE_OUTER_BOUND ( 'NONE', #997, .T. ) ;
#3602 = CARTESIAN_POINT ( 'NONE',  ( -8.121558582316792396, -23.74999999999999645, 3.550687472877651629 ) ) ;
#3603 = CARTESIAN_POINT ( 'NONE',  ( -2.076833265075072266, -8.407161531158021006, 2.383492984350220389 ) ) ;
#3604 = EDGE_LOOP ( 'NONE', ( #7927, #20325, #18564, #7685 ) ) ;
#3605 = CARTESIAN_POINT ( 'NONE',  ( -12.63478567848856571, -19.00582323632600890, 4.762720106674273701 ) ) ;
#3606 = CARTESIAN_POINT ( 'NONE',  ( -6.527808582316794173, -23.72900456129165647, 4.275561207030568411 ) ) ;
#3607 = CARTESIAN_POINT ( 'NONE',  ( -7.190941417683176518, -23.27327832286946219, 4.701595411283453707 ) ) ;
#3608 = ORIENTED_EDGE ( 'NONE', *, *, #16361, .F. ) ;
#3609 = CARTESIAN_POINT ( 'NONE',  ( 13.38007464613909470, -19.24373036997283037, 4.743072998953621777 ) ) ;
#3610 = CARTESIAN_POINT ( 'NONE',  ( -11.00000000000000000, -23.70993649053891517, 5.466506350946108483 ) ) ;
#3611 = ORIENTED_EDGE ( 'NONE', *, *, #19595, .F. ) ;
#3612 = VERTEX_POINT ( 'NONE', #13963 ) ;
#3613 = CARTESIAN_POINT ( 'NONE',  ( 7.499999999999999112, -18.49999999999999645, 4.000000000000000000 ) ) ;
#3614 = EDGE_CURVE ( 'NONE', #6794, #5732, #20369, .T. ) ;
#3615 = VECTOR ( 'NONE', #2888, 999.9999999999998863 ) ;
#3616 = ORIENTED_EDGE ( 'NONE', *, *, #7346, .F. ) ;
#3617 = LINE ( 'NONE', #18057, #16443 ) ;
#3618 = B_SPLINE_CURVE_WITH_KNOTS ( 'NONE', 3,
 ( #878, #18458, #15410, #9237, #7473, #12265 ),
 .UNSPECIFIED., .F., .F.,
 ( 4, 2, 4 ),
 ( 0.000000000000000000, 0.5000000000000000000, 1.000000000000000000 ),
 .UNSPECIFIED. ) ;
#3619 = VERTEX_POINT ( 'NONE', #19420 ) ;
#3620 = LINE ( 'NONE', #19439, #13333 ) ;
#3621 = CARTESIAN_POINT ( 'NONE',  ( 6.813547257480585095, 10.00000000000000000, 1.000000000000000000 ) ) ;
#3622 = FACE_OUTER_BOUND ( 'NONE', #19252, .T. ) ;
#3623 = CARTESIAN_POINT ( 'NONE',  ( -18.98630159782011262, 4.999999999999999112, 0.000000000000000000 ) ) ;
#3624 = CARTESIAN_POINT ( 'NONE',  ( -5.121558582316794173, -23.74999999999999645, 3.550687472877651629 ) ) ;
#3625 = AXIS2_PLACEMENT_3D ( 'NONE', #12521, #3215, #4676 ) ;
#3626 = EDGE_CURVE ( 'NONE', #14595, #14589, #17623, .T. ) ;
#3627 = AXIS2_PLACEMENT_3D ( 'NONE', #20137, #20336, #10710 ) ;
#3628 = DIRECTION ( 'NONE',  ( 0.000000000000000000, 0.000000000000000000, 1.000000000000000000 ) ) ;
#3629 = CARTESIAN_POINT ( 'NONE',  ( 9.347191417683177406, -21.22443879296941915, 1.770995438708345748 ) ) ;
#3630 = DIRECTION ( 'NONE',  ( 0.000000000000000000, -1.000000000000000000, 0.000000000000000000 ) ) ;
#3631 = CARTESIAN_POINT ( 'NONE',  ( -9.722191417683177406, -21.02099543870834353, 3.964901035250761208 ) ) ;
#3632 = CARTESIAN_POINT ( 'NONE',  ( -7.465308582316796837, -19.47900456129164937, 4.484846433055089676 ) ) ;
#3633 = VERTEX_POINT ( 'NONE', #4967 ) ;
#3634 = CARTESIAN_POINT ( 'NONE',  ( 12.62499999999998224, -20.24999999999998934, 4.166666666666636765 ) ) ;
#3635 = CARTESIAN_POINT ( 'NONE',  ( -12.62499999998404121, -20.24999999996810729, 2.793053905886972998 ) ) ;
#3636 = ORIENTED_EDGE ( 'NONE', *, *, #18506, .T. ) ;
#3637 = CARTESIAN_POINT ( 'NONE',  ( 3.469446951953523943E-14, 10.00000000000009592, 1.000000000000000000 ) ) ;
#3638 = EDGE_CURVE ( 'NONE', #6239, #8745, #14485, .T. ) ;
#3639 = DIRECTION ( 'NONE',  ( 0.000000000000000000, -1.000000000000000000, 0.000000000000000000 ) ) ;
#3640 = EDGE_CURVE ( 'NONE', #18418, #19600, #6646, .T. ) ;
#3641 = ORIENTED_EDGE ( 'NONE', *, *, #4872, .T. ) ;
#3642 = VECTOR ( 'NONE', #4756, 1000.000000000000000 ) ;
#3643 = SHAPE_DEFINITION_REPRESENTATION ( #5005, #6161 ) ;
#3644 = ORIENTED_EDGE ( 'NONE', *, *, #9219, .T. ) ;
#3645 = VECTOR ( 'NONE', #12844, 1000.000000000000000 ) ;
#3646 = LINE ( 'NONE', #11592, #10131 ) ;
#3647 = EDGE_LOOP ( 'NONE', ( #8554, #1181, #6661, #10410, #15244, #274, #11069, #4006, #580, #16277 ) ) ;
#3648 = LINE ( 'NONE', #14737, #13937 ) ;
#3649 = CARTESIAN_POINT ( 'NONE',  ( 12.74043380832193684, -14.42059267975384529, 5.611358176248560703 ) ) ;
#3650 = DIRECTION ( 'NONE',  ( 1.000000000000000000, 0.000000000000000000, 0.000000000000000000 ) ) ;
#3651 = EDGE_CURVE ( 'NONE', #2288, #11536, #6336, .T. ) ;
#3652 = CARTESIAN_POINT ( 'NONE',  ( 12.69247507894198712, -16.84250851341299082, 5.559274842915185033 ) ) ;
#3653 = CARTESIAN_POINT ( 'NONE',  ( -2.499999999999998668, -24.49999999999999289, 4.000000000000000000 ) ) ;
#3654 = VECTOR ( 'NONE', #16460, 1000.000000000000000 ) ;
#3655 = CARTESIAN_POINT ( 'NONE',  ( 9.996558582316795949, -22.05068747287764452, 0.9999999999999978906 ) ) ;
#3656 = CARTESIAN_POINT ( 'NONE',  ( -12.62499999999998224, -20.25000000000006395, 4.416666666666681174 ) ) ;
#3657 = CARTESIAN_POINT ( 'NONE',  ( -12.53469141768317741, -19.47900456129164581, 2.515153566944927199 ) ) ;
#3658 = AXIS2_PLACEMENT_3D ( 'NONE', #5342, #17799, #16015 ) ;
#3659 = CARTESIAN_POINT ( 'NONE',  ( 0.000000000000000000, 9.000000000000001776, 0.000000000000000000 ) ) ;
#3660 = CARTESIAN_POINT ( 'NONE',  ( 26.04469207716615031, 9.000000000000001776, 1.000000000000000000 ) ) ;
#3661 = CARTESIAN_POINT ( 'NONE',  ( 11.68405858231679595, -21.32873467460644079, 2.757051763020455404 ) ) ;
#3662 = EDGE_CURVE ( 'NONE', #20379, #13564, #9476, .T. ) ;
#3663 = CARTESIAN_POINT ( 'NONE',  ( -9.440941417683177406, -20.72672167713052715, 2.298404588716546293 ) ) ;
#3664 = ORIENTED_EDGE ( 'NONE', *, *, #3786, .F. ) ;
#3665 = EDGE_CURVE ( 'NONE', #13753, #10392, #12812, .T. ) ;
#3666 = VERTEX_POINT ( 'NONE', #15944 ) ;
#3667 = CARTESIAN_POINT ( 'NONE',  ( 13.85343352903393388, 3.910893216212274925, 5.991044282956552891 ) ) ;
#3668 = DIRECTION ( 'NONE',  ( 1.734723475976809560E-16, -1.000000000000000000, 0.000000000000000000 ) ) ;
#3669 = CARTESIAN_POINT ( 'NONE',  ( -11.74178095869206828, 4.999999999999999112, 1.000000000000000000 ) ) ;
#3670 = EDGE_LOOP ( 'NONE', ( #7744, #19537, #16011, #18474 ) ) ;
#3671 = LINE ( 'NONE', #746, #2096 ) ;
#3672 = VECTOR ( 'NONE', #7591, 1000.000000000000000 ) ;
#3673 = LINE ( 'NONE', #11824, #11367 ) ;
#3674 = CARTESIAN_POINT ( 'NONE',  ( 13.12500000000000533, 4.265117264764102245, 4.000000000000000888 ) ) ;
#3675 = CARTESIAN_POINT ( 'NONE',  ( 13.49014615398506045, -14.43511922376608680, 5.596513032956658584 ) ) ;
#3676 = CARTESIAN_POINT ( 'NONE',  ( 0.000000000000000000, 16.00000000000000000, 1.000000000000000000 ) ) ;
#3677 = CARTESIAN_POINT ( 'NONE',  ( 3.317048600639548095, -9.800042196285016161, 2.741212564741740465 ) ) ;
#3678 = AXIS2_PLACEMENT_3D ( 'NONE', #1230, #10749, #20686 ) ;
#3679 = ADVANCED_FACE ( 'NONE', ( #8315 ), #20674, .T. ) ;
#3680 = VECTOR ( 'NONE', #1930, 1000.000000000000000 ) ;
#3681 = CARTESIAN_POINT ( 'NONE',  ( 8.876396343307449754, 11.64110105645932691, 10.00000000000000000 ) ) ;
#3682 = CARTESIAN_POINT ( 'NONE',  ( -12.62499999999998224, -19.49999999999998934, 4.166666666666637653 ) ) ;
#3683 = CARTESIAN_POINT ( 'NONE',  ( 9.621558582316794173, -23.74999999999999645, 3.550687472877651629 ) ) ;
#3684 = DIRECTION ( 'NONE',  ( -0.000000000000000000, -0.000000000000000000, -1.000000000000000000 ) ) ;
#3685 = CARTESIAN_POINT ( 'NONE',  ( 12.95145221759166354, -3.764163011652346569, 5.840524842913703552 ) ) ;
#3686 = CARTESIAN_POINT ( 'NONE',  ( -1.619022621591186928, -9.864917468222230923, 2.372643865078341019 ) ) ;
#3687 = CARTESIAN_POINT ( 'NONE',  ( 7.746558582316795949, -21.94931252712234127, 4.499999999999999112 ) ) ;
#3688 = VECTOR ( 'NONE', #16770, 1000.000000000000000 ) ;
#3689 = CARTESIAN_POINT ( 'NONE',  ( 8.597191417683177406, -22.77556120703057729, 5.229004561291655584 ) ) ;
#3690 = CARTESIAN_POINT ( 'NONE',  ( -6.621558582316796837, -22.99999999999999645, 3.550687472877652073 ) ) ;
#3691 = ORIENTED_EDGE ( 'NONE', *, *, #8097, .F. ) ;
#3692 = CARTESIAN_POINT ( 'NONE',  ( 13.89992416064626646, 5.508670112635706495, 5.888743936161951353 ) ) ;
#3693 = CARTESIAN_POINT ( 'NONE',  ( 13.12529397354238192, 5.014845663890295846, 3.000000000000000000 ) ) ;
#3694 = VECTOR ( 'NONE', #12043, 1000.000000000000000 ) ;
#3695 = CARTESIAN_POINT ( 'NONE',  ( -3.500698171653725765, 0.000000000000000000, 1.000000000000000000 ) ) ;
#3696 = AXIS2_PLACEMENT_3D ( 'NONE', #20370, #20480, #18692 ) ;
#3697 = ORIENTED_EDGE ( 'NONE', *, *, #7459, .F. ) ;
#3698 = EDGE_LOOP ( 'NONE', ( #10786, #8846, #17765, #2870 ) ) ;
#3699 = DIRECTION ( 'NONE',  ( -0.000000000000000000, -0.000000000000000000, -1.000000000000000000 ) ) ;
#3700 = DIRECTION ( 'NONE',  ( 1.000000000000000000, -0.000000000000000000, 0.000000000000000000 ) ) ;
#3701 = B_SPLINE_CURVE_WITH_KNOTS ( 'NONE', 3,
 ( #11551, #14889, #3600, #5585, #7163, #6948, #14793, #14991, #3811, #13215, #5171, #17931, #13423, #7059, #19829, #13526, #5482, #9979, #16559, #18247, #11755, #3910, #16362, #13318, #2038, #6846, #19718, #10290, #15100, #472, #18146, #10189 ),
 .UNSPECIFIED., .F., .F.,
 ( 4, 2, 2, 2, 1, 2, 2, 2, 2, 2, 2, 2, 1, 2, 2, 2, 4 ),
 ( 0.000000000000000000, 0.06250846311920765785, 0.09376269467881148678, 0.1093898104586116665, 0.1172033683485095151, 0.1211101472934592721, 0.1250169262384090152, 0.1875253893575668795, 0.2500338524767247161, 0.3125423155958825805, 0.3437965471554634833, 0.3594236629352539625, 0.3672372208251511450, 0.3711439997701008187, 0.3750507787150505479, 0.4375592418342420520, 0.5000677049534336671 ),
 .UNSPECIFIED. ) ;
#3702 = CARTESIAN_POINT ( 'NONE',  ( -24.50000000000000000, 3.000000000000000888, 1.000000000000000000 ) ) ;
#3703 = CARTESIAN_POINT ( 'NONE',  ( 22.56633994409548194, 0.000000000000000000, 1.000000000000000000 ) ) ;
#3704 = CARTESIAN_POINT ( 'NONE',  ( 1.655860418491166941, -9.114909740826840689, 2.372641880528837621 ) ) ;
#3705 = FACE_OUTER_BOUND ( 'NONE', #10422, .T. ) ;
#3706 = AXIS2_PLACEMENT_3D ( 'NONE', #14944, #19474, #320 ) ;
#3707 = DIRECTION ( 'NONE',  ( 1.000000000000000000, 0.000000000000000000, 0.000000000000000000 ) ) ;
#3708 = VECTOR ( 'NONE', #7576, 1000.000000000000000 ) ;
#3709 = EDGE_CURVE ( 'NONE', #20470, #17483, #12709, .T. ) ;
#3710 = DIRECTION ( 'NONE',  ( 0.000000000000000000, -1.000000000000000000, 0.000000000000000000 ) ) ;
#3711 = CARTESIAN_POINT ( 'NONE',  ( -2.109407804498405703, -9.207748739546751438, 2.396484790045401603 ) ) ;
#3712 = CARTESIAN_POINT ( 'NONE',  ( -10.74655858231679417, -21.94931252712234482, 5.250000000000000888 ) ) ;
#3713 = VECTOR ( 'NONE', #15793, 1000.000000000000000 ) ;
#3714 = AXIS2_PLACEMENT_3D ( 'NONE', #9689, #5187, #6660 ) ;
#3715 = CARTESIAN_POINT ( 'NONE',  ( -1.619022621591186928, -8.364917468222230923, 2.372643865078341019 ) ) ;
#3716 = VERTEX_POINT ( 'NONE', #3503 ) ;
#3717 = CARTESIAN_POINT ( 'NONE',  ( -12.99447614883396973, -0.8414544838704021146, 5.153345106674984244 ) ) ;
#3718 = CARTESIAN_POINT ( 'NONE',  ( -9.621558582316794173, -23.74999999999999645, 3.550687472877651629 ) ) ;
#3719 = CARTESIAN_POINT ( 'NONE',  ( -5.784691417683179182, -23.77099543870834353, 4.174186261275252718 ) ) ;
#3720 = VERTEX_POINT ( 'NONE', #12600 ) ;
#3721 = CARTESIAN_POINT ( 'NONE',  ( 13.84501469867711698, 4.235742283194553259, 4.333333333333380999 ) ) ;
#3722 = ORIENTED_EDGE ( 'NONE', *, *, #6216, .F. ) ;
#3723 = ORIENTED_EDGE ( 'NONE', *, *, #4954, .F. ) ;
#3724 = LINE ( 'NONE', #484, #13722 ) ;
#3725 = VERTEX_POINT ( 'NONE', #19111 ) ;
#3726 = DIRECTION ( 'NONE',  ( 1.000000000000000000, 0.000000000000000000, 0.000000000000000000 ) ) ;
#3727 = AXIS2_PLACEMENT_3D ( 'NONE', #19572, #6901, #13269 ) ;
#3728 = EDGE_LOOP ( 'NONE', ( #17200, #16705, #11798, #9456 ) ) ;
#3729 = CARTESIAN_POINT ( 'NONE',  ( 7.659691417683176518, -22.67418626127524917, 1.729004561291651587 ) ) ;
#3730 = DIRECTION ( 'NONE',  ( 0.000000000000000000, -1.000000000000000000, 0.000000000000000000 ) ) ;
#3731 = DIRECTION ( 'NONE',  ( -0.000000000000000000, -0.000000000000000000, -1.000000000000000000 ) ) ;
#3732 = CARTESIAN_POINT ( 'NONE',  ( 11.00000000000000000, -23.83493649053891517, 4.999999999999999112 ) ) ;
#3733 = CARTESIAN_POINT ( 'NONE',  ( 12.00000000000000178, -18.50000000000000355, 4.000000000000000000 ) ) ;
#3734 = ADVANCED_FACE ( 'NONE', ( #16264 ), #14831, .T. ) ;
#3735 = CARTESIAN_POINT ( 'NONE',  ( 13.86676110481170632, 3.833935792988865110, 6.739421935864088553 ) ) ;
#3736 = CARTESIAN_POINT ( 'NONE',  ( 22.56633994409548194, 10.00000000000000000, 1.000000000000000000 ) ) ;
#3737 = CARTESIAN_POINT ( 'NONE',  ( 7.565941417683176518, -23.20159541128344927, 2.226721677130534705 ) ) ;
#3738 = DIRECTION ( 'NONE',  ( 0.000000000000000000, 1.000000000000000000, -0.000000000000000000 ) ) ;
#3739 = CARTESIAN_POINT ( 'NONE',  ( -8.972191417683177406, -22.97900456129165292, 3.035098964749240125 ) ) ;
#3740 = AXIS2_PLACEMENT_3D ( 'NONE', #17989, #11404, #10244 ) ;
#3741 = CARTESIAN_POINT ( 'NONE',  ( -9.621558582316795949, -24.50000000000000000, 3.550687472877651629 ) ) ;
#3742 = VERTEX_POINT ( 'NONE', #14896 ) ;
#3743 = EDGE_CURVE ( 'NONE', #7302, #9844, #574, .T. ) ;
#3744 = CARTESIAN_POINT ( 'NONE',  ( 13.10372118337080849, 3.925419760224517329, 6.005889426248455010 ) ) ;
#3745 = CARTESIAN_POINT ( 'NONE',  ( -12.62500000000001954, -20.24999999999450040, 3.833333333368183382 ) ) ;
#3746 = ORIENTED_EDGE ( 'NONE', *, *, #6940, .T. ) ;
#3747 = EDGE_CURVE ( 'NONE', #1300, #8663, #4225, .T. ) ;
#3748 = DIRECTION ( 'NONE',  ( 0.000000000000000000, 0.000000000000000000, -1.000000000000000000 ) ) ;
#3749 = DIRECTION ( 'NONE',  ( -1.000000000000000000, 0.000000000000000000, 0.000000000000000000 ) ) ;
#3750 = PRESENTATION_LAYER_ASSIGNMENT (  '', '', ( #12756 ) ) ;
#3751 = VERTEX_POINT ( 'NONE', #6113 ) ;
#3752 = VERTEX_POINT ( 'NONE', #9345 ) ;
#3753 = CARTESIAN_POINT ( 'NONE',  ( -11.00000000000000000, -23.83493649053891517, 5.249999999999999112 ) ) ;
#3754 = VERTEX_POINT ( 'NONE', #986 ) ;
#3755 = CARTESIAN_POINT ( 'NONE',  ( 23.60856191738414012, 9.000000000000001776, 1.000000000000000000 ) ) ;
#3756 = VECTOR ( 'NONE', #6331, 1000.000000000000000 ) ;
#3757 = CARTESIAN_POINT ( 'NONE',  ( 13.10431844137356627, 3.955581289335645234, 6.006545679920360925 ) ) ;
#3758 = CARTESIAN_POINT ( 'NONE',  ( -1.948765222931501784, -9.143197003266354983, 1.629906614618163552 ) ) ;
#3759 = CARTESIAN_POINT ( 'NONE',  ( -14.49999999999998579, -19.49999999999999645, 1.000000000000000000 ) ) ;
#3760 = CARTESIAN_POINT ( 'NONE',  ( -18.69064177244175795, 0.000000000000000000, 1.000000000000000000 ) ) ;
#3761 = EDGE_CURVE ( 'NONE', #12230, #5259, #10507, .T. ) ;
#3762 = CARTESIAN_POINT ( 'NONE',  ( 12.62499999999998224, -20.24999999999991829, 4.333333333333343695 ) ) ;
#3763 = CARTESIAN_POINT ( 'NONE',  ( -23.35856191738413656, 0.000000000000000000, 1.000000000000000000 ) ) ;
#3764 = CARTESIAN_POINT ( 'NONE',  ( 9.902808582316795949, -23.08622137881038938, 1.020995438708339309 ) ) ;
#3765 = CARTESIAN_POINT ( 'NONE',  ( -12.62499999999998224, -20.24999999999998934, 4.291666666666698937 ) ) ;
#3766 = CARTESIAN_POINT ( 'NONE',  ( -9.347191417683177406, -20.91377862118959285, 1.020995438708345082 ) ) ;
#3767 = CARTESIAN_POINT ( 'NONE',  ( -16.62779268661489951, 10.00000000000000000, 1.000000000000000000 ) ) ;
#3768 = PLANE ( 'NONE',  #1073 ) ;
#3769 = AXIS2_PLACEMENT_3D ( 'NONE', #9130, #2434, #5887 ) ;
#3770 = CARTESIAN_POINT ( 'NONE',  ( 10.65280858231679595, -21.53509896474924901, 4.479004561291659137 ) ) ;
#3771 = DIRECTION ( 'NONE',  ( -0.000000000000000000, -1.000000000000000000, -0.000000000000000000 ) ) ;
#3772 = VERTEX_POINT ( 'NONE', #7375 ) ;
#3773 = EDGE_LOOP ( 'NONE', ( #763, #19842, #10079, #12431, #16955 ) ) ;
#3774 = CARTESIAN_POINT ( 'NONE',  ( 13.39902456816392906, -19.03675930772010361, 5.497554699623231400 ) ) ;
#3775 = DIRECTION ( 'NONE',  ( 0.000000000000000000, 0.000000000000000000, -1.000000000000000000 ) ) ;
#3776 = CARTESIAN_POINT ( 'NONE',  ( 5.000000000000000000, -12.50000000000000000, 1.000000000000000000 ) ) ;
#3777 = EDGE_LOOP ( 'NONE', ( #966, #3225, #1660, #17269 ) ) ;
#3778 = EDGE_CURVE ( 'NONE', #18372, #5957, #10606, .T. ) ;
#3779 = DIRECTION ( 'NONE',  ( 1.000000000000000000, 2.312964634635756072E-15, 0.000000000000000000 ) ) ;
#3780 = CARTESIAN_POINT ( 'NONE',  ( 11.49178095869207006, 0.000000000000000000, 1.000000000000000000 ) ) ;
#3781 = FACE_OUTER_BOUND ( 'NONE', #11056, .T. ) ;
#3782 = CARTESIAN_POINT ( 'NONE',  ( 13.43259567872942917, -17.34141822415733714, 5.534013032956523581 ) ) ;
#3783 = CARTESIAN_POINT ( 'NONE',  ( -3.997260319564023501, 0.000000000000000000, 1.000000000000000000 ) ) ;
#3784 = CARTESIAN_POINT ( 'NONE',  ( 1.126276606324276619, -8.364917468222230923, 2.372643865078341019 ) ) ;
#3785 = AXIS2_PLACEMENT_3D ( 'NONE', #4645, #18788, #11039 ) ;
#3786 = EDGE_CURVE ( 'NONE', #999, #7456, #15722, .T. ) ;
#3787 = EDGE_CURVE ( 'NONE', #17877, #19250, #1199, .T. ) ;
#3788 = DIRECTION ( 'NONE',  ( 1.000000000000000000, 0.000000000000000000, -0.000000000000000000 ) ) ;
#3789 = CARTESIAN_POINT ( 'NONE',  ( -12.78345773956433895, -11.49788415197707181, 4.924178440007425550 ) ) ;
#3790 = CARTESIAN_POINT ( 'NONE',  ( 5.121558582316794173, -23.74999999999999645, 3.550687472877651629 ) ) ;
#3791 = CARTESIAN_POINT ( 'NONE',  ( -9.805650798910056309, 0.000000000000000000, 1.000000000000000000 ) ) ;
#3792 = CARTESIAN_POINT ( 'NONE',  ( 13.10372118337080849, 3.925419760224517329, 6.005889426248455010 ) ) ;
#3793 = CARTESIAN_POINT ( 'NONE',  ( -15.61404127825609223, 0.000000000000000000, 0.000000000000000000 ) ) ;
#3794 = CARTESIAN_POINT ( 'NONE',  ( 9.902808582316795949, -22.46490103525074034, 2.520995438708341307 ) ) ;
#3795 = CARTESIAN_POINT ( 'NONE',  ( 7.378441417683176518, -23.74999999999999645, 3.449312527122335492 ) ) ;
#3796 = CARTESIAN_POINT ( 'NONE',  ( -8.402808582316794173, -22.77556120703056308, 1.770995438708339975 ) ) ;
#3797 = VERTEX_POINT ( 'NONE', #1098 ) ;
#3798 = CARTESIAN_POINT ( 'NONE',  ( 12.67103257592000176, -18.67535491604046172, 6.269892079155907183 ) ) ;
#3799 = CARTESIAN_POINT ( 'NONE',  ( 12.62499999999998224, -19.49999999999998934, 4.166666666666637653 ) ) ;
#3800 = DIRECTION ( 'NONE',  ( -0.000000000000000000, -0.8660254037844363761, 0.5000000000000041078 ) ) ;
#3801 = ORIENTED_EDGE ( 'NONE', *, *, #1988, .T. ) ;
#3802 = EDGE_CURVE ( 'NONE', #2580, #14057, #10825, .T. ) ;
#3803 = ORIENTED_EDGE ( 'NONE', *, *, #9135, .F. ) ;
#3804 = DIRECTION ( 'NONE',  ( 0.7071067811865475727, 0.000000000000000000, -0.7071067811865475727 ) ) ;
#3805 = DIRECTION ( 'NONE',  ( -1.000000000000000000, 0.000000000000000000, 0.000000000000000000 ) ) ;
#3806 = CARTESIAN_POINT ( 'NONE',  ( 20.50349085826861995, 10.00000000000000000, 1.000000000000000000 ) ) ;
#3807 = DIRECTION ( 'NONE',  ( 1.000000000000000000, -0.000000000000000000, 0.000000000000000000 ) ) ;
#3808 = CARTESIAN_POINT ( 'NONE',  ( 2.623717082130370137, -10.12934627674766830, 2.633169448359191644 ) ) ;
#3809 = PLANE ( 'NONE',  #3139 ) ;
#3810 = LINE ( 'NONE', #16261, #4708 ) ;
#3811 = CARTESIAN_POINT ( 'NONE',  ( 12.71979495292231910, -20.49936819972870694, 3.538210221529994648 ) ) ;
#3812 = DIRECTION ( 'NONE',  ( 0.000000000000000000, -0.000000000000000000, 1.000000000000000000 ) ) ;
#3813 = CARTESIAN_POINT ( 'NONE',  ( -9.152808582316794173, -21.22443879296942626, 5.229004561291659137 ) ) ;
#3814 = CARTESIAN_POINT ( 'NONE',  ( -3.607313482701580476, -10.70492285834919244, 2.223603995567122293 ) ) ;
#3815 = ORIENTED_EDGE ( 'NONE', *, *, #12646, .T. ) ;
#3816 = CARTESIAN_POINT ( 'NONE',  ( -13.47561960997282071, -14.41870969638424071, 4.846833296715798767 ) ) ;
#3817 = CARTESIAN_POINT ( 'NONE',  ( -7.746558582316794173, -21.94931252712234482, 5.250000000000000888 ) ) ;
#3818 = CARTESIAN_POINT ( 'NONE',  ( -4.940941417683177406, -20.72672167713052715, 2.298404588716546293 ) ) ;
#3819 = ORIENTED_EDGE ( 'NONE', *, *, #11460, .F. ) ;
#3820 = CARTESIAN_POINT ( 'NONE',  ( 13.39482594849551944, -19.24878960097397140, 5.493002502378098839 ) ) ;
#3821 = DIRECTION ( 'NONE',  ( -1.000000000000000000, 0.000000000000000000, 0.000000000000000000 ) ) ;
#3822 = ORIENTED_EDGE ( 'NONE', *, *, #4238, .F. ) ;
#3823 = VERTEX_POINT ( 'NONE', #12483 ) ;
#3824 = ADVANCED_FACE ( 'NONE', ( #13939 ), #15515, .T. ) ;
#3825 = FACE_OUTER_BOUND ( 'NONE', #867, .T. ) ;
#3826 = VECTOR ( 'NONE', #19876, 1000.000000000000000 ) ;
#3827 = ORIENTED_EDGE ( 'NONE', *, *, #7357, .F. ) ;
#3828 = DIRECTION ( 'NONE',  ( 1.000000000000000000, 0.000000000000000000, 0.000000000000000000 ) ) ;
#3829 = ORIENTED_EDGE ( 'NONE', *, *, #2577, .F. ) ;
#3830 = DIRECTION ( 'NONE',  ( 0.000000000000000000, -0.000000000000000000, 1.000000000000000000 ) ) ;
#3831 = FACE_OUTER_BOUND ( 'NONE', #4590, .T. ) ;
#3832 = FACE_OUTER_BOUND ( 'NONE', #3363, .T. ) ;
#3833 = CARTESIAN_POINT ( 'NONE',  ( 3.779650890485476200, -11.92851441922421607, 2.537846752097290715 ) ) ;
#3834 = CARTESIAN_POINT ( 'NONE',  ( -7.746558582316794173, -21.94931252712234482, 5.250000000000000888 ) ) ;
#3835 = CARTESIAN_POINT ( 'NONE',  ( 12.62500000000002132, -20.99999999999450395, 3.833333333368183382 ) ) ;
#3836 = DIRECTION ( 'NONE',  ( -0.000000000000000000, -0.000000000000000000, -1.000000000000000000 ) ) ;
#3837 = CARTESIAN_POINT ( 'NONE',  ( 9.722191417683177406, -21.02099543870834353, 3.964901035250761208 ) ) ;
#3838 = CARTESIAN_POINT ( 'NONE',  ( -6.815941417683177406, -21.32873467460645145, 4.242948236979555254 ) ) ;
#3839 = CARTESIAN_POINT ( 'NONE',  ( -6.059058582316795949, -20.19639159124062999, 5.231925497173373074 ) ) ;
#3840 = VERTEX_POINT ( 'NONE', #20142 ) ;
#3841 = CARTESIAN_POINT ( 'NONE',  ( 12.62499999999998579, -20.24999999999999289, 3.666666666666653640 ) ) ;
#3842 = CARTESIAN_POINT ( 'NONE',  ( -12.62515553039088090, -20.24214571525854467, 4.629702272822510345 ) ) ;
#3843 = ORIENTED_EDGE ( 'NONE', *, *, #8470, .F. ) ;
#3844 = DIRECTION ( 'NONE',  ( 0.000000000000000000, 0.000000000000000000, 1.000000000000000000 ) ) ;
#3845 = DIRECTION ( 'NONE',  ( -0.4999999999999947820, -0.8660254037844415942, 0.000000000000000000 ) ) ;
#3846 = VECTOR ( 'NONE', #20364, 1000.000000000000000 ) ;
#3847 = ORIENTED_EDGE ( 'NONE', *, *, #5836, .T. ) ;
#3848 = ORIENTED_EDGE ( 'NONE', *, *, #4115, .F. ) ;
#3849 = EDGE_CURVE ( 'NONE', #17667, #3253, #6208, .T. ) ;
#3850 = CARTESIAN_POINT ( 'NONE',  ( 13.21006596862446969, -19.93552635338812706, 3.471618140591925084 ) ) ;
#3851 = VECTOR ( 'NONE', #538, 1000.000000000000000 ) ;
#3852 = ORIENTED_EDGE ( 'NONE', *, *, #12470, .T. ) ;
#3853 = LINE ( 'NONE', #3952, #11642 ) ;
#3854 = CARTESIAN_POINT ( 'NONE',  ( 12.83635126708105823, -9.576761012430582198, 5.715524842913705328 ) ) ;
#3855 = EDGE_CURVE ( 'NONE', #14060, #17851, #39, .T. ) ;
#3856 = CARTESIAN_POINT ( 'NONE',  ( -3.059891148793807414, -12.07002330923453570, 2.381574079220715401 ) ) ;
#3857 = DIRECTION ( 'NONE',  ( -0.000000000000000000, -0.000000000000000000, 1.000000000000000000 ) ) ;
#3858 = DIRECTION ( 'NONE',  ( -0.1736481776669309696, -0.9848077530122080203, 0.000000000000000000 ) ) ;
#3859 = ADVANCED_FACE ( 'NONE', ( #2867 ), #18876, .T. ) ;
#3860 = FACE_OUTER_BOUND ( 'NONE', #18577, .T. ) ;
#3861 = CARTESIAN_POINT ( 'NONE',  ( -14.49999999999998579, -18.49999999999999645, 4.000000000000000000 ) ) ;
#3862 = CARTESIAN_POINT ( 'NONE',  ( 6.152808582316795949, -20.91377862118960351, 5.979004561291660913 ) ) ;
#3863 = CARTESIAN_POINT ( 'NONE',  ( -12.66849571425264287, -18.05346643024382303, 5.533233176248494978 ) ) ;
#3864 = CARTESIAN_POINT ( 'NONE',  ( -7.565941417683177406, -23.73192549717336064, 1.696391591240623331 ) ) ;
#3865 = VERTEX_POINT ( 'NONE', #10922 ) ;
#3866 = CARTESIAN_POINT ( 'NONE',  ( 13.09030858231679417, -21.32581373872472597, 1.729004561291657582 ) ) ;
#3867 = LINE ( 'NONE', #10148, #6079 ) ;
#3868 = CARTESIAN_POINT ( 'NONE',  ( 11.02780858231679595, -22.97900456129165647, 3.964901035250747885 ) ) ;
#3869 = CARTESIAN_POINT ( 'NONE',  ( 16.37779268661489596, 10.00000000000000000, 1.000000000000000000 ) ) ;
#3870 = ORIENTED_EDGE ( 'NONE', *, *, #15979, .T. ) ;
#3871 = EDGE_LOOP ( 'NONE', ( #2528, #78, #7484, #15377 ) ) ;
#3872 = CARTESIAN_POINT ( 'NONE',  ( 13.40621837757088564, -18.67347193267085714, 5.505367199623145247 ) ) ;
#3873 = PLANE ( 'NONE',  #422 ) ;
#3874 = PRESENTATION_STYLE_ASSIGNMENT (( #16839 ) ) ;
#3875 = VERTEX_POINT ( 'NONE', #15306 ) ;
#3876 = EDGE_CURVE ( 'NONE', #9549, #10573, #20341, .T. ) ;
#3877 = DIRECTION ( 'NONE',  ( 0.000000000000000000, 1.000000000000000000, -0.000000000000000000 ) ) ;
#3878 = CARTESIAN_POINT ( 'NONE',  ( -5.433390479346035029, 9.000000000000001776, 1.000000000000000000 ) ) ;
#3879 = DIRECTION ( 'NONE',  ( 1.000000000000000000, 0.000000000000000000, 0.000000000000000000 ) ) ;
#3880 = CARTESIAN_POINT ( 'NONE',  ( 13.37524505148396514, -20.23762490005974968, 4.659512268729234741 ) ) ;
#3881 = DIRECTION ( 'NONE',  ( 1.000000000000000000, 0.000000000000000000, -0.000000000000000000 ) ) ;
#3882 = CARTESIAN_POINT ( 'NONE',  ( 2.445888733774860935, -8.532121313016713060, 2.415585152653916712 ) ) ;
#3883 = DIRECTION ( 'NONE',  ( 1.000000000000000000, 0.000000000000000000, 0.000000000000000000 ) ) ;
#3884 = CARTESIAN_POINT ( 'NONE',  ( -13.12529397354238192, 5.014845663890295846, 4.666666666666619889 ) ) ;
#3885 = CARTESIAN_POINT ( 'NONE',  ( 5.965308582316793284, -20.22900456129164937, 4.174186261275266929 ) ) ;
#3886 = FACE_OUTER_BOUND ( 'NONE', #6170, .T. ) ;
#3887 = CARTESIAN_POINT ( 'NONE',  ( 12.62562019941893432, -20.21867992933967173, 4.757612834768309540 ) ) ;
#3888 = ADVANCED_FACE ( 'NONE', ( #9044 ), #15415, .T. ) ;
#3889 = CARTESIAN_POINT ( 'NONE',  ( -2.534747216115884161, -9.671180236796224960, 2.515503256513427210 ) ) ;
#3890 = CARTESIAN_POINT ( 'NONE',  ( 7.559058582316795949, -21.25705176302045274, 4.171265325393551215 ) ) ;
#3891 = CARTESIAN_POINT ( 'NONE',  ( 7.003441417683177406, -22.05068747287765873, 5.250000000000000888 ) ) ;
#3892 =( BOUNDED_SURFACE ( )  B_SPLINE_SURFACE ( 3, 3, ( 
 ( #9503, #499, #6680, #3841, #1864, #2168, #3634, #8151, #10016, #10124, #8457, #8552, #19450, #11487, #1764, #16395, #8246, #6879, #4998, #2073, #14824, #14514, #19646, #290, #3435, #14612, #191, #17767, #13049, #14723, #6574, #14922, #16199, #11679, #13153, #5107, #13248, #6783, #3536, #9813, #5305, #600, #16496, #17866, #19755, #5205, #9912, #16293, #1965, #18077, #8348, #6986, #401, #19550, #5415, #16095, #11583, #3744, #13355, #11788, #17963, #12939, #18179, #19343, #11377, #13770, #812, #5515, #18592, #2266, #5930, #10537, #10637, #8867, #7295, #11993, #7509, #8655, #15027, #2475, #18391, #20068, #17012, #13872, #2689, #11887 ),
 ( #19863, #20272, #20173, #708, #5733, #15337, #4256, #16698, #15447, #5833, #12202, #7196, #16589, #9076, #1131, #7094, #2578, #4054, #10438, #16807, #10221, #13558, #13459, #18279, #909, #12303, #10329, #3942, #18699, #4155, #16907, #2376, #13658, #8766, #15137, #19959, #1018, #8963, #5619, #15236, #12104, #18493, #7408, #1532, #10952, #17318, #7605, #9578, #10748, #6040, #12608, #20487, #18909, #14386, #6237, #15952, #4772, #20685, #4666, #4567, #15853, #14079, #12716, #6456, #3108, #17120, #69, #19119, #3003, #2800, #6142, #3207, #9378, #12512, #1334, #13972, #11057, #14177, #4472, #9174, #15549, #17430, #20585, #7815, #1634, #9484 ),
 ( #19012, #7912, #11157, #10856, #8016, #14275, #6347, #7711, #1229, #17527, #12819, #20377, #4365, #15753, #1436, #12411, #18806, #17220, #2898, #9273, #15647, #14901, #19319, #169, #11251, #6553, #379, #3609, #9992, #6857, #14590, #19429, #19219, #3411, #577, #2050, #16372, #9792, #6957, #4976, #5281, #6763, #17630, #13132, #13226, #11560, #11658, #1841, #265, #4873, #19530, #11356, #8435, #8126, #5182, #17941, #3304, #14804, #16177, #12916, #17745, #9685, #8226, #6656, #17845, #16072, #14492, #19623, #1743, #13026, #481, #18051, #3510, #16271, #5085, #16475, #11464, #9891, #1940, #8324, #14698, #3721, #2148, #10099, #8529, #18565 ),
 ( #2661, #2553, #11764, #8844, #18468, #7380, #19839, #4230, #16882, #8939, #10302, #19729, #13744, #20146, #10199, #5706, #788, #15111, #7173, #13330, #16673, #5390, #18156, #4027, #9050, #13434, #15002, #3820, #683, #15211, #4130, #10511, #992, #8742, #13536, #16568, #18258, #15419, #15310, #5806, #3920, #1104, #5491, #12177, #887, #2245, #7272, #10611, #12077, #16983, #2349, #19938, #8631, #13633, #11864, #7069, #5596, #20042, #11966, #18366, #10411, #16783, #2451, #13943, #12276, #9151, #6010, #6117, #18668, #6314, #7580, #3083, #4542, #20345, #14154, #18880, #15618, #15519, #20561, #14247, #1506, #9248, #11132, #17291, #1204, #2871 ),
 ( #20657, #17195, #12386, #17501, #7482, #20460, #6212, #12583, #12689, #10926, #13843, #19091, #9555, #1410, #11031, #18779, #4745, #10829, #1301, #20246, #7791, #4446, #18983, #17094, #4639, #17402, #5904, #9457, #7683, #14052, #12488, #4338, #2973, #9350, #15729, #10721, #3181, #15829, #7888, #15928, #2771, #8298, #12999, #9766, #3278, #14672, #8411, #16346, #3388, #5254, #11437, #9657, #17717, #1719, #6739, #14568, #14778, #11329, #8103, #11631, #1605, #241, #352, #13104, #455, #19402, #7986, #6833, #3692, #16248, #5158, #12893, #17606, #9964, #14358, #18021, #1917, #2021, #6630, #5060, #16152, #19601, #44, #6429, #17821, #1816 ),
 ( #19507, #3488, #9864, #13202, #11537, #10076, #17916, #3583, #8202, #12793, #19195, #4848, #11229, #16044, #14467, #146, #6532, #19297, #4950, #8505, #18443, #12048, #18232, #2221, #16757, #15082, #3999, #16545, #10385, #7042, #764, #8820, #16858, #15187, #3798, #4105, #864, #2322, #8604, #2428, #14975, #5677, #7247, #13299, #19700, #10488, #2525, #16450, #7150, #13609, #2124, #16642, #13513, #552, #5363, #19915, #20013, #14876, #6932, #10175, #653, #5569, #11741, #18133, #13410, #19815, #18336, #5469, #11841, #11940, #3895, #10274, #8711, #8367, #418, #14426, #17882, #6591, #8166, #18097, #5219, #13166, #16111, #14532, #19663, #6895 ),
 ( #311, #17674, #5325, #109, #1779, #1981, #9827, #8262, #3762, #16309, #11699, #14840, #10034, #14742, #14628, #11597, #3450, #2088, #16513, #19566, #6495, #10140, #8473, #6696, #12856, #16213, #13264, #19467, #1881, #11397, #3347, #6798, #3549, #207, #19258, #4911, #17982, #9928, #3652, #2185, #16413, #11289, #5122, #515, #13068, #11502, #9726, #12959, #19360, #5017, #17782, #18294, #5433, #4354, #13861, #7004, #6133, #20477, #15437, #13475, #18795, #10739, #20366, #7112, #6028, #3957, #17109, #10846, #10940, #17209, #15043, #12502, #2886, #12292, #19878, #4461, #5532, #14068, #9264, #11806, #18195, #4557, #17308, #8568, #18687, #15635 ) ),
 .UNSPECIFIED., .T., .F., .F. ) 
 B_SPLINE_SURFACE_WITH_KNOTS ( ( 4, 3, 4 ),
 ( 4, 2, 2, 2, 2, 2, 2, 2, 2, 2, 2, 2, 2, 2, 2, 2, 2, 2, 2, 2, 2, 2, 2, 2, 2, 2, 2, 2, 2, 2, 2, 2, 2, 2, 2, 2, 2, 2, 2, 2, 2, 2, 4 ),
 ( 0.000000000000000000, 0.5000000000000000000, 1.000000000000000000 ),
 ( 0.000000000000000000, 0.03481082764294501225, 0.05122453910963481460, 0.05943139484297971231, 0.06353482270965216117, 0.06763825057632461002, 0.07081696859385246123, 0.07399568661138031245, 0.08035312264643601488, 0.09306799471654741973, 0.1057828667866588246, 0.1121403028217145270, 0.1153190208392423644, 0.1184977388567702156, 0.1214804596100246270, 0.1244631803632790246, 0.1304286218697878197, 0.1423595048828054099, 0.1662212709088405904, 0.2139448029609109514, 0.3093918670650516733, 0.5002859952733331728, 0.6911801234816146167, 0.7866271875857553386, 0.8343507196378256996, 0.8582124856638608801, 0.8701433686768784703, 0.8761088101833873765, 0.8790915309366418295, 0.8820742516898961716, 0.8853411830926052328, 0.8886081144953141830, 0.8951419773007323055, 0.9082097029115685505, 0.9212774285224047954, 0.9278112913278229179, 0.9310782227305318681, 0.9343451541332409294, 0.9384485819999133227, 0.9425520098665858271, 0.9507588655999306138, 0.9671725770666204092, 1.000000000000000000 ),
 .UNSPECIFIED. ) 
 GEOMETRIC_REPRESENTATION_ITEM ( )  RATIONAL_B_SPLINE_SURFACE ( (
 ( 1.000000000000000000, 1.000000000000000000, 1.000000000000000000, 1.000000000000000000, 1.000000000000000000, 1.000000000000000000, 1.000000000000000000, 1.000000000000000000, 1.000000000000000000, 1.000000000000000000, 1.000000000000000000, 1.000000000000000000, 1.000000000000000000, 1.000000000000000000, 1.000000000000000000, 1.000000000000000000, 1.000000000000000000, 1.000000000000000000, 1.000000000000000000, 1.000000000000000000, 1.000000000000000000, 1.000000000000000000, 1.000000000000000000, 1.000000000000000000, 1.000000000000000000, 1.000000000000000000, 1.000000000000000000, 1.000000000000000000, 1.000000000000000000, 1.000000000000000000, 1.000000000000000000, 1.000000000000000000, 1.000000000000000000, 1.000000000000000000, 1.000000000000000000, 1.000000000000000000, 1.000000000000000000, 1.000000000000000000, 1.000000000000000000, 1.000000000000000000, 1.000000000000000000, 1.000000000000000000, 1.000000000000000000, 1.000000000000000000, 1.000000000000000000, 1.000000000000000000, 1.000000000000000000, 1.000000000000000000, 1.000000000000000000, 1.000000000000000000, 1.000000000000000000, 1.000000000000000000, 1.000000000000000000, 1.000000000000000000, 1.000000000000000000, 1.000000000000000000, 1.000000000000000000, 1.000000000000000000, 1.000000000000000000, 1.000000000000000000, 1.000000000000000000, 1.000000000000000000, 1.000000000000000000, 1.000000000000000000, 1.000000000000000000, 1.000000000000000000, 1.000000000000000000, 1.000000000000000000, 1.000000000000000000, 1.000000000000000000, 1.000000000000000000, 1.000000000000000000, 1.000000000000000000, 1.000000000000000000, 1.000000000000000000, 1.000000000000000000, 1.000000000000000000, 1.000000000000000000, 1.000000000000000000, 1.000000000000000000, 1.000000000000000000, 1.000000000000000000, 1.000000000000000000, 1.000000000000000000, 1.000000000000000000, 1.000000000000000000),
 ( 0.3333333333333333703, 0.3333333333333333703, 0.3333333333333333703, 0.3333333333333333703, 0.3333333333333333703, 0.3333333333333333703, 0.3333333333333333703, 0.3333333333333333703, 0.3333333333333333703, 0.3333333333333333703, 0.3333333333333333703, 0.3333333333333333703, 0.3333333333333333703, 0.3333333333333333703, 0.3333333333333333703, 0.3333333333333333703, 0.3333333333333333703, 0.3333333333333333703, 0.3333333333333333703, 0.3333333333333333703, 0.3333333333333333703, 0.3333333333333333703, 0.3333333333333333703, 0.3333333333333333703, 0.3333333333333333703, 0.3333333333333333703, 0.3333333333333333703, 0.3333333333333333703, 0.3333333333333333703, 0.3333333333333333703, 0.3333333333333333703, 0.3333333333333333703, 0.3333333333333333703, 0.3333333333333333703, 0.3333333333333333703, 0.3333333333333333703, 0.3333333333333333703, 0.3333333333333333703, 0.3333333333333333703, 0.3333333333333333703, 0.3333333333333333703, 0.3333333333333333703, 0.3333333333333333703, 0.3333333333333333703, 0.3333333333333333703, 0.3333333333333333703, 0.3333333333333333703, 0.3333333333333333703, 0.3333333333333333703, 0.3333333333333333703, 0.3333333333333333703, 0.3333333333333333703, 0.3333333333333333703, 0.3333333333333333703, 0.3333333333333333703, 0.3333333333333333703, 0.3333333333333333703, 0.3333333333333333703, 0.3333333333333333703, 0.3333333333333333703, 0.3333333333333333703, 0.3333333333333333703, 0.3333333333333333703, 0.3333333333333333703, 0.3333333333333333703, 0.3333333333333333703, 0.3333333333333333703, 0.3333333333333333703, 0.3333333333333333703, 0.3333333333333333703, 0.3333333333333333703, 0.3333333333333333703, 0.3333333333333333703, 0.3333333333333333703, 0.3333333333333333703, 0.3333333333333333703, 0.3333333333333333703, 0.3333333333333333703, 0.3333333333333333703, 0.3333333333333333703, 0.3333333333333333703, 0.3333333333333333703, 0.3333333333333333703, 0.3333333333333333703, 0.3333333333333333703, 0.3333333333333333703),
 ( 0.3333333333333333703, 0.3333333333333333703, 0.3333333333333333703, 0.3333333333333333703, 0.3333333333333333703, 0.3333333333333333703, 0.3333333333333333703, 0.3333333333333333703, 0.3333333333333333703, 0.3333333333333333703, 0.3333333333333333703, 0.3333333333333333703, 0.3333333333333333703, 0.3333333333333333703, 0.3333333333333333703, 0.3333333333333333703, 0.3333333333333333703, 0.3333333333333333703, 0.3333333333333333703, 0.3333333333333333703, 0.3333333333333333703, 0.3333333333333333703, 0.3333333333333333703, 0.3333333333333333703, 0.3333333333333333703, 0.3333333333333333703, 0.3333333333333333703, 0.3333333333333333703, 0.3333333333333333703, 0.3333333333333333703, 0.3333333333333333703, 0.3333333333333333703, 0.3333333333333333703, 0.3333333333333333703, 0.3333333333333333703, 0.3333333333333333703, 0.3333333333333333703, 0.3333333333333333703, 0.3333333333333333703, 0.3333333333333333703, 0.3333333333333333703, 0.3333333333333333703, 0.3333333333333333703, 0.3333333333333333703, 0.3333333333333333703, 0.3333333333333333703, 0.3333333333333333703, 0.3333333333333333703, 0.3333333333333333703, 0.3333333333333333703, 0.3333333333333333703, 0.3333333333333333703, 0.3333333333333333703, 0.3333333333333333703, 0.3333333333333333703, 0.3333333333333333703, 0.3333333333333333703, 0.3333333333333333703, 0.3333333333333333703, 0.3333333333333333703, 0.3333333333333333703, 0.3333333333333333703, 0.3333333333333333703, 0.3333333333333333703, 0.3333333333333333703, 0.3333333333333333703, 0.3333333333333333703, 0.3333333333333333703, 0.3333333333333333703, 0.3333333333333333703, 0.3333333333333333703, 0.3333333333333333703, 0.3333333333333333703, 0.3333333333333333703, 0.3333333333333333703, 0.3333333333333333703, 0.3333333333333333703, 0.3333333333333333703, 0.3333333333333333703, 0.3333333333333333703, 0.3333333333333333703, 0.3333333333333333703, 0.3333333333333333703, 0.3333333333333333703, 0.3333333333333333703, 0.3333333333333333703),
 ( 1.000000000000000000, 1.000000000000000000, 1.000000000000000000, 1.000000000000000000, 1.000000000000000000, 1.000000000000000000, 1.000000000000000000, 1.000000000000000000, 1.000000000000000000, 1.000000000000000000, 1.000000000000000000, 1.000000000000000000, 1.000000000000000000, 1.000000000000000000, 1.000000000000000000, 1.000000000000000000, 1.000000000000000000, 1.000000000000000000, 1.000000000000000000, 1.000000000000000000, 1.000000000000000000, 1.000000000000000000, 1.000000000000000000, 1.000000000000000000, 1.000000000000000000, 1.000000000000000000, 1.000000000000000000, 1.000000000000000000, 1.000000000000000000, 1.000000000000000000, 1.000000000000000000, 1.000000000000000000, 1.000000000000000000, 1.000000000000000000, 1.000000000000000000, 1.000000000000000000, 1.000000000000000000, 1.000000000000000000, 1.000000000000000000, 1.000000000000000000, 1.000000000000000000, 1.000000000000000000, 1.000000000000000000, 1.000000000000000000, 1.000000000000000000, 1.000000000000000000, 1.000000000000000000, 1.000000000000000000, 1.000000000000000000, 1.000000000000000000, 1.000000000000000000, 1.000000000000000000, 1.000000000000000000, 1.000000000000000000, 1.000000000000000000, 1.000000000000000000, 1.000000000000000000, 1.000000000000000000, 1.000000000000000000, 1.000000000000000000, 1.000000000000000000, 1.000000000000000000, 1.000000000000000000, 1.000000000000000000, 1.000000000000000000, 1.000000000000000000, 1.000000000000000000, 1.000000000000000000, 1.000000000000000000, 1.000000000000000000, 1.000000000000000000, 1.000000000000000000, 1.000000000000000000, 1.000000000000000000, 1.000000000000000000, 1.000000000000000000, 1.000000000000000000, 1.000000000000000000, 1.000000000000000000, 1.000000000000000000, 1.000000000000000000, 1.000000000000000000, 1.000000000000000000, 1.000000000000000000, 1.000000000000000000, 1.000000000000000000),
 ( 0.3333333333333333703, 0.3333333333333333703, 0.3333333333333333703, 0.3333333333333333703, 0.3333333333333333703, 0.3333333333333333703, 0.3333333333333333703, 0.3333333333333333703, 0.3333333333333333703, 0.3333333333333333703, 0.3333333333333333703, 0.3333333333333333703, 0.3333333333333333703, 0.3333333333333333703, 0.3333333333333333703, 0.3333333333333333703, 0.3333333333333333703, 0.3333333333333333703, 0.3333333333333333703, 0.3333333333333333703, 0.3333333333333333703, 0.3333333333333333703, 0.3333333333333333703, 0.3333333333333333703, 0.3333333333333333703, 0.3333333333333333703, 0.3333333333333333703, 0.3333333333333333703, 0.3333333333333333703, 0.3333333333333333703, 0.3333333333333333703, 0.3333333333333333703, 0.3333333333333333703, 0.3333333333333333703, 0.3333333333333333703, 0.3333333333333333703, 0.3333333333333333703, 0.3333333333333333703, 0.3333333333333333703, 0.3333333333333333703, 0.3333333333333333703, 0.3333333333333333703, 0.3333333333333333703, 0.3333333333333333703, 0.3333333333333333703, 0.3333333333333333703, 0.3333333333333333703, 0.3333333333333333703, 0.3333333333333333703, 0.3333333333333333703, 0.3333333333333333703, 0.3333333333333333703, 0.3333333333333333703, 0.3333333333333333703, 0.3333333333333333703, 0.3333333333333333703, 0.3333333333333333703, 0.3333333333333333703, 0.3333333333333333703, 0.3333333333333333703, 0.3333333333333333703, 0.3333333333333333703, 0.3333333333333333703, 0.3333333333333333703, 0.3333333333333333703, 0.3333333333333333703, 0.3333333333333333703, 0.3333333333333333703, 0.3333333333333333703, 0.3333333333333333703, 0.3333333333333333703, 0.3333333333333333703, 0.3333333333333333703, 0.3333333333333333703, 0.3333333333333333703, 0.3333333333333333703, 0.3333333333333333703, 0.3333333333333333703, 0.3333333333333333703, 0.3333333333333333703, 0.3333333333333333703, 0.3333333333333333703, 0.3333333333333333703, 0.3333333333333333703, 0.3333333333333333703, 0.3333333333333333703),
 ( 0.3333333333333333703, 0.3333333333333333703, 0.3333333333333333703, 0.3333333333333333703, 0.3333333333333333703, 0.3333333333333333703, 0.3333333333333333703, 0.3333333333333333703, 0.3333333333333333703, 0.3333333333333333703, 0.3333333333333333703, 0.3333333333333333703, 0.3333333333333333703, 0.3333333333333333703, 0.3333333333333333703, 0.3333333333333333703, 0.3333333333333333703, 0.3333333333333333703, 0.3333333333333333703, 0.3333333333333333703, 0.3333333333333333703, 0.3333333333333333703, 0.3333333333333333703, 0.3333333333333333703, 0.3333333333333333703, 0.3333333333333333703, 0.3333333333333333703, 0.3333333333333333703, 0.3333333333333333703, 0.3333333333333333703, 0.3333333333333333703, 0.3333333333333333703, 0.3333333333333333703, 0.3333333333333333703, 0.3333333333333333703, 0.3333333333333333703, 0.3333333333333333703, 0.3333333333333333703, 0.3333333333333333703, 0.3333333333333333703, 0.3333333333333333703, 0.3333333333333333703, 0.3333333333333333703, 0.3333333333333333703, 0.3333333333333333703, 0.3333333333333333703, 0.3333333333333333703, 0.3333333333333333703, 0.3333333333333333703, 0.3333333333333333703, 0.3333333333333333703, 0.3333333333333333703, 0.3333333333333333703, 0.3333333333333333703, 0.3333333333333333703, 0.3333333333333333703, 0.3333333333333333703, 0.3333333333333333703, 0.3333333333333333703, 0.3333333333333333703, 0.3333333333333333703, 0.3333333333333333703, 0.3333333333333333703, 0.3333333333333333703, 0.3333333333333333703, 0.3333333333333333703, 0.3333333333333333703, 0.3333333333333333703, 0.3333333333333333703, 0.3333333333333333703, 0.3333333333333333703, 0.3333333333333333703, 0.3333333333333333703, 0.3333333333333333703, 0.3333333333333333703, 0.3333333333333333703, 0.3333333333333333703, 0.3333333333333333703, 0.3333333333333333703, 0.3333333333333333703, 0.3333333333333333703, 0.3333333333333333703, 0.3333333333333333703, 0.3333333333333333703, 0.3333333333333333703, 0.3333333333333333703),
 ( 1.000000000000000000, 1.000000000000000000, 1.000000000000000000, 1.000000000000000000, 1.000000000000000000, 1.000000000000000000, 1.000000000000000000, 1.000000000000000000, 1.000000000000000000, 1.000000000000000000, 1.000000000000000000, 1.000000000000000000, 1.000000000000000000, 1.000000000000000000, 1.000000000000000000, 1.000000000000000000, 1.000000000000000000, 1.000000000000000000, 1.000000000000000000, 1.000000000000000000, 1.000000000000000000, 1.000000000000000000, 1.000000000000000000, 1.000000000000000000, 1.000000000000000000, 1.000000000000000000, 1.000000000000000000, 1.000000000000000000, 1.000000000000000000, 1.000000000000000000, 1.000000000000000000, 1.000000000000000000, 1.000000000000000000, 1.000000000000000000, 1.000000000000000000, 1.000000000000000000, 1.000000000000000000, 1.000000000000000000, 1.000000000000000000, 1.000000000000000000, 1.000000000000000000, 1.000000000000000000, 1.000000000000000000, 1.000000000000000000, 1.000000000000000000, 1.000000000000000000, 1.000000000000000000, 1.000000000000000000, 1.000000000000000000, 1.000000000000000000, 1.000000000000000000, 1.000000000000000000, 1.000000000000000000, 1.000000000000000000, 1.000000000000000000, 1.000000000000000000, 1.000000000000000000, 1.000000000000000000, 1.000000000000000000, 1.000000000000000000, 1.000000000000000000, 1.000000000000000000, 1.000000000000000000, 1.000000000000000000, 1.000000000000000000, 1.000000000000000000, 1.000000000000000000, 1.000000000000000000, 1.000000000000000000, 1.000000000000000000, 1.000000000000000000, 1.000000000000000000, 1.000000000000000000, 1.000000000000000000, 1.000000000000000000, 1.000000000000000000, 1.000000000000000000, 1.000000000000000000, 1.000000000000000000, 1.000000000000000000, 1.000000000000000000, 1.000000000000000000, 1.000000000000000000, 1.000000000000000000, 1.000000000000000000, 1.000000000000000000) ) ) 
 REPRESENTATION_ITEM ( '' )  SURFACE ( )  );
#3893 = CARTESIAN_POINT ( 'NONE',  ( -12.62155858231679417, -23.74999999999999645, 3.550687472877651629 ) ) ;
#3894 = ORIENTED_EDGE ( 'NONE', *, *, #3407, .F. ) ;
#3895 = CARTESIAN_POINT ( 'NONE',  ( 13.15384296923648400, 5.706569946443514674, 5.461568745250741763 ) ) ;
#3896 = CARTESIAN_POINT ( 'NONE',  ( 12.72590726430969532, -14.40418315237199742, 4.861678440007700885 ) ) ;
#3897 = VECTOR ( 'NONE', #11948, 1000.000000000000000 ) ;
#3898 = CARTESIAN_POINT ( 'NONE',  ( 0.000000000000000000, 4.999999999999999112, 1.000000000000000000 ) ) ;
#3899 = ORIENTED_EDGE ( 'NONE', *, *, #10755, .F. ) ;
#3900 = ADVANCED_FACE ( 'NONE', ( #5900 ), #12270, .T. ) ;
#3901 = ORIENTED_EDGE ( 'NONE', *, *, #11498, .F. ) ;
#3902 = EDGE_CURVE ( 'NONE', #14893, #4330, #20456, .T. ) ;
#3903 = LINE ( 'NONE', #16552, #5443 ) ;
#3904 = DIRECTION ( 'NONE',  ( 0.000000000000000000, 0.000000000000000000, -1.000000000000000000 ) ) ;
#3905 = CARTESIAN_POINT ( 'NONE',  ( -7.500000000000000000, -23.83493649053891517, 5.249999999999999112 ) ) ;
#3906 = LINE ( 'NONE', #13211, #19685 ) ;
#3907 = CARTESIAN_POINT ( 'NONE',  ( 1.904508877737772998, -9.138371295333994837, 2.378667276417936627 ) ) ;
#3908 = FACE_OUTER_BOUND ( 'NONE', #19980, .T. ) ;
#3909 = CARTESIAN_POINT ( 'NONE',  ( 10.93924542913430820, 11.64110105645932691, 0.000000000000000000 ) ) ;
#3910 = CARTESIAN_POINT ( 'NONE',  ( 13.23867574658679303, -20.53938148496870042, 3.467514063319057982 ) ) ;
#3911 = CARTESIAN_POINT ( 'NONE',  ( -1.797604806073912709, -9.120796646272857799, 2.374153755450133740 ) ) ;
#3912 = CARTESIAN_POINT ( 'NONE',  ( -6.246558582316794173, -21.94931252712234482, 5.250000000000000888 ) ) ;
#3913 = CARTESIAN_POINT ( 'NONE',  ( -2.616191246582922680, -8.630616848980537270, 2.440880773935528048 ) ) ;
#3914 = ORIENTED_EDGE ( 'NONE', *, *, #2703, .T. ) ;
#3915 = CARTESIAN_POINT ( 'NONE',  ( -13.38929389708972195, -18.77815819697223887, 4.753083296715700179 ) ) ;
#3916 = CARTESIAN_POINT ( 'NONE',  ( -5.309058582316794173, -23.27327832286945153, 2.298404588716537411 ) ) ;
#3917 = CARTESIAN_POINT ( 'NONE',  ( 8.496558582316795949, -22.05068747287764452, 0.9999999999999978906 ) ) ;
#3918 = CARTESIAN_POINT ( 'NONE',  ( -7.940941417683175629, -21.25705176302044208, 2.828734674606458555 ) ) ;
#3919 = ORIENTED_EDGE ( 'NONE', *, *, #1049, .F. ) ;
#3920 = CARTESIAN_POINT ( 'NONE',  ( 13.49014615398506045, -14.43511922376608680, 5.596513032956658584 ) ) ;
#3921 = PLANE ( 'NONE',  #5714 ) ;
#3922 = VERTEX_POINT ( 'NONE', #17089 ) ;
#3923 = ORIENTED_EDGE ( 'NONE', *, *, #8620, .F. ) ;
#3924 = LINE ( 'NONE', #2354, #19802 ) ;
#3925 = ORIENTED_EDGE ( 'NONE', *, *, #5034, .F. ) ;
#3926 = DIRECTION ( 'NONE',  ( 1.000000000000000000, 0.000000000000000000, 0.000000000000000000 ) ) ;
#3927 = VERTEX_POINT ( 'NONE', #2767 ) ;
#3928 = CARTESIAN_POINT ( 'NONE',  ( 4.565941417683176518, -23.20159541128344927, 2.226721677130534705 ) ) ;
#3929 = LINE ( 'NONE', #20053, #6664 ) ;
#3930 = DIRECTION ( 'NONE',  ( 1.000000000000000000, 0.000000000000000000, 0.000000000000000000 ) ) ;
#3931 = CARTESIAN_POINT ( 'NONE',  ( 3.336296098497695262, -9.936854405034125648, 2.776348673047012383 ) ) ;
#3932 = FACE_OUTER_BOUND ( 'NONE', #14417, .T. ) ;
#3933 = ADVANCED_FACE ( 'NONE', ( #9145 ), #6005, .T. ) ;
#3934 = CARTESIAN_POINT ( 'NONE',  ( 13.89730118381875279, 5.376209782841177898, 6.083536567043803522 ) ) ;
#3935 = LINE ( 'NONE', #493, #20664 ) ;
#3936 = CARTESIAN_POINT ( 'NONE',  ( 9.159691417683175629, -22.36352608949543352, 2.479004561291652031 ) ) ;
#3937 = CARTESIAN_POINT ( 'NONE',  ( -12.64323021897839006, -19.32937394158751943, 5.504219675487169283 ) ) ;
#3938 = CARTESIAN_POINT ( 'NONE',  ( -7.190941417683177406, -22.74294823697955081, 4.171265325393542334 ) ) ;
#3939 = CARTESIAN_POINT ( 'NONE',  ( -10.94094141768317741, -20.19639159124061933, 1.768074502826635586 ) ) ;
#3940 = VECTOR ( 'NONE', #9905, 1000.000000000000000 ) ;
#3941 = VERTEX_POINT ( 'NONE', #17396 ) ;
#3942 = CARTESIAN_POINT ( 'NONE',  ( 12.63036675113625407, -19.22897906761645004, 4.757923088130392664 ) ) ;
#3943 = CARTESIAN_POINT ( 'NONE',  ( -13.12512971825177033, 5.006550771716304915, 5.133277049491872468 ) ) ;
#3944 = VERTEX_POINT ( 'NONE', #19293 ) ;
#3945 = VECTOR ( 'NONE', #4277, 1000.000000000000000 ) ;
#3946 = LINE ( 'NONE', #19962, #8281 ) ;
#3947 = CARTESIAN_POINT ( 'NONE',  ( 11.00000000000000000, -20.16506350946107418, 5.000000000000000000 ) ) ;
#3948 = ORIENTED_EDGE ( 'NONE', *, *, #2086, .T. ) ;
#3949 = ORIENTED_EDGE ( 'NONE', *, *, #7074, .F. ) ;
#3950 = VECTOR ( 'NONE', #17641, 1000.000000000000000 ) ;
#3951 = ORIENTED_EDGE ( 'NONE', *, *, #20374, .F. ) ;
#3952 = CARTESIAN_POINT ( 'NONE',  ( -21.42243175760212637, 0.000000000000000000, 1.000000000000000000 ) ) ;
#3953 = DIRECTION ( 'NONE',  ( 0.000000000000000000, 0.000000000000000000, 1.000000000000000000 ) ) ;
#3954 = CARTESIAN_POINT ( 'NONE',  ( -3.502569552650398155, -9.961070227720959736, 2.032567780072621400 ) ) ;
#3955 = FACE_OUTER_BOUND ( 'NONE', #9914, .T. ) ;
#3956 = LINE ( 'NONE', #10965, #16041 ) ;
#3957 = CARTESIAN_POINT ( 'NONE',  ( 13.11514659413808737, 4.502403003978772134, 5.887634658581065494 ) ) ;
#3958 = LINE ( 'NONE', #13785, #17366 ) ;
#3959 = CARTESIAN_POINT ( 'NONE',  ( 10.09719141768317741, -23.08622137881040359, 5.979004561291654696 ) ) ;
#3960 = CARTESIAN_POINT ( 'NONE',  ( -13.09293046926041626, 3.380488697651010011, 5.994170676248444352 ) ) ;
#3961 = CARTESIAN_POINT ( 'NONE',  ( -8.315941417683177406, -20.26807450282663225, 5.303608408759377113 ) ) ;
#3962 = EDGE_CURVE ( 'NONE', #8358, #6555, #17735, .T. ) ;
#3963 = ORIENTED_EDGE ( 'NONE', *, *, #150, .T. ) ;
#3964 = DIRECTION ( 'NONE',  ( -0.000000000000000000, 0.000000000000000000, -1.000000000000000000 ) ) ;
#3965 = DIRECTION ( 'NONE',  ( 0.000000000000000000, -0.5000000000000041078, -0.8660254037844363761 ) ) ;
#3966 = CARTESIAN_POINT ( 'NONE',  ( -13.79242507427300879, 0.07996625081441015304, 6.658692769197546824 ) ) ;
#3967 = AXIS2_PLACEMENT_3D ( 'NONE', #12061, #772, #873 ) ;
#3968 = AXIS2_PLACEMENT_3D ( 'NONE', #14284, #6359, #18064 ) ;
#3969 = CARTESIAN_POINT ( 'NONE',  ( 4.934058582316795061, -22.67126532539354855, 4.242948236979545484 ) ) ;
#3970 = LINE ( 'NONE', #838, #1324 ) ;
#3971 = AXIS2_PLACEMENT_3D ( 'NONE', #16432, #19797, #11925 ) ;
#3972 = ORIENTED_EDGE ( 'NONE', *, *, #6354, .F. ) ;
#3973 = ORIENTED_EDGE ( 'NONE', *, *, #6288, .F. ) ;
#3974 = CARTESIAN_POINT ( 'NONE',  ( 13.39296152110871851, -19.34294318400601753, 5.489418334493660012 ) ) ;
#3975 = ADVANCED_FACE ( 'NONE', ( #1812 ), #18978, .F. ) ;
#3976 = VECTOR ( 'NONE', #2484, 1000.000000000000000 ) ;
#3977 = PLANE ( 'NONE',  #14104 ) ;
#3978 = FILL_AREA_STYLE_COLOUR ( '', #19719 ) ;
#3979 = VERTEX_POINT ( 'NONE', #11127 ) ;
#3980 = CARTESIAN_POINT ( 'NONE',  ( 13.50000000000000178, 7.806255641895631925E-15, 2.000000000000000000 ) ) ;
#3981 = CARTESIAN_POINT ( 'NONE',  ( 0.000000000000000000, 4.999999999999999112, 1.000000000000000000 ) ) ;
#3982 = DIRECTION ( 'NONE',  ( 0.000000000000000000, -1.000000000000000000, 0.000000000000000000 ) ) ;
#3983 = CARTESIAN_POINT ( 'NONE',  ( 13.41341218697771609, -18.31018455762212227, 5.513179699623425023 ) ) ;
#3984 = CIRCLE ( 'NONE', #9331, 10.00000000000000000 ) ;
#3985 = DIRECTION ( 'NONE',  ( 1.000000000000000000, 0.000000000000000000, 0.000000000000000000 ) ) ;
#3986 = CARTESIAN_POINT ( 'NONE',  ( 2.616191246582922680, -8.630616848980537270, 2.440880773935528048 ) ) ;
#3987 = VECTOR ( 'NONE', #14617, 1000.000000000000000 ) ;
#3988 = PLANE ( 'NONE',  #20089 ) ;
#3989 = CARTESIAN_POINT ( 'NONE',  ( -13.12529397353891270, 5.014845663890295846, 3.333333333333220239 ) ) ;
#3990 = DIRECTION ( 'NONE',  ( 0.000000000000000000, -0.000000000000000000, -1.000000000000000000 ) ) ;
#3991 = CARTESIAN_POINT ( 'NONE',  ( 12.62155858231679417, -23.74999999999999645, 3.550687472877651629 ) ) ;
#3992 = CARTESIAN_POINT ( 'NONE',  ( -13.86316420010827777, 3.652292105464413297, 6.735515685864076119 ) ) ;
#3993 = EDGE_CURVE ( 'NONE', #14460, #12662, #3484, .T. ) ;
#3994 = CARTESIAN_POINT ( 'NONE',  ( -14.49999999999998579, -19.49999999999999645, 4.000000000000000000 ) ) ;
#3995 = CARTESIAN_POINT ( 'NONE',  ( 11.59030858231679417, -21.32581373872472597, 1.729004561291657582 ) ) ;
#3996 = CARTESIAN_POINT ( 'NONE',  ( 10.00344141768317563, -22.05068747287765873, 5.250000000000000888 ) ) ;
#3997 = CARTESIAN_POINT ( 'NONE',  ( -12.90280858231679773, -22.77556120703056308, 1.770995438708339975 ) ) ;
#3998 = ORIENTED_EDGE ( 'NONE', *, *, #6286, .T. ) ;
#3999 = CARTESIAN_POINT ( 'NONE',  ( 12.65816212372154403, -19.32531275206247301, 6.255900543948403225 ) ) ;
#4000 = EDGE_CURVE ( 'NONE', #1851, #18752, #12683, .T. ) ;
#4001 = CARTESIAN_POINT ( 'NONE',  ( 12.62499994688180749, -19.50000268246798640, 4.473800639250938183 ) ) ;
#4002 = EDGE_CURVE ( 'NONE', #4902, #3922, #16147, .T. ) ;
#4003 = CARTESIAN_POINT ( 'NONE',  ( -0.000000000000000000, 11.64110105645932691, 0.000000000000000000 ) ) ;
#4004 = ORIENTED_EDGE ( 'NONE', *, *, #10270, .F. ) ;
#4005 = VECTOR ( 'NONE', #12253, 1000.000000000000000 ) ;
#4006 = ORIENTED_EDGE ( 'NONE', *, *, #13739, .F. ) ;
#4007 = DIRECTION ( 'NONE',  ( -1.000000000000000000, 0.000000000000000000, 0.000000000000000000 ) ) ;
#4008 = VECTOR ( 'NONE', #5945, 1000.000000000000000 ) ;
#4009 = CARTESIAN_POINT ( 'NONE',  ( 2.687849085826861995, 11.64110105645932691, 0.000000000000000000 ) ) ;
#4010 = DIRECTION ( 'NONE',  ( -1.000000000000000000, 0.000000000000000000, 0.000000000000000000 ) ) ;
#4011 = CARTESIAN_POINT ( 'NONE',  ( 5.000000000000000000, -12.50000000000000000, 1.000000000000000000 ) ) ;
#4012 = CARTESIAN_POINT ( 'NONE',  ( 1.732184490400474175, -9.869581059509965115, 2.373841568485653308 ) ) ;
#4013 = CARTESIAN_POINT ( 'NONE',  ( 13.87470602645761808, 4.985154336109792972, 4.000000000000000000 ) ) ;
#4014 = LINE ( 'NONE', #877, #5736 ) ;
#4015 = EDGE_CURVE ( 'NONE', #2409, #8973, #19397, .T. ) ;
#4016 = AXIS2_PLACEMENT_3D ( 'NONE', #11717, #19274, #8486 ) ;
#4017 = FACE_OUTER_BOUND ( 'NONE', #20255, .T. ) ;
#4018 = CARTESIAN_POINT ( 'NONE',  ( -10.55905858231679595, -20.72672167713054137, 4.701595411283463477 ) ) ;
#4019 = CARTESIAN_POINT ( 'NONE',  ( -2.121089610268797276, -8.411987239090384705, 1.634732322550447758 ) ) ;
#4020 = ORIENTED_EDGE ( 'NONE', *, *, #8876, .F. ) ;
#4021 = CARTESIAN_POINT ( 'NONE',  ( -13.53317008522746434, -11.51241069598931510, 4.909333296715523431 ) ) ;
#4022 = CARTESIAN_POINT ( 'NONE',  ( -9.059058582316794173, -20.72672167713054137, 4.701595411283463477 ) ) ;
#4023 = VECTOR ( 'NONE', #12979, 1000.000000000000000 ) ;
#4024 = CARTESIAN_POINT ( 'NONE',  ( 12.80905858231679417, -23.80360840875935935, 1.768074502826626260 ) ) ;
#4025 = CARTESIAN_POINT ( 'NONE',  ( -11.69094141768317741, -22.74294823697955081, 4.171265325393542334 ) ) ;
#4026 = VERTEX_POINT ( 'NONE', #6625 ) ;
#4027 = CARTESIAN_POINT ( 'NONE',  ( 13.39107665282975645, -19.43812903209671461, 5.476542851584349947 ) ) ;
#4028 = LINE ( 'NONE', #9051, #13052 ) ;
#4029 = ORIENTED_EDGE ( 'NONE', *, *, #18173, .T. ) ;
#4030 = ORIENTED_EDGE ( 'NONE', *, *, #6057, .T. ) ;
#4031 = PLANE ( 'NONE',  #17417 ) ;
#4032 = ORIENTED_EDGE ( 'NONE', *, *, #1886, .F. ) ;
#4033 = CARTESIAN_POINT ( 'NONE',  ( -13.38800411018677572, -19.59329243556743805, 5.436267741224407146 ) ) ;
#4034 = EDGE_CURVE ( 'NONE', #4780, #1844, #14563, .T. ) ;
#4035 = VECTOR ( 'NONE', #17061, 1000.000000000000000 ) ;
#4036 = ORIENTED_EDGE ( 'NONE', *, *, #7162, .F. ) ;
#4037 = AXIS2_PLACEMENT_3D ( 'NONE', #4447, #4543, #7684 ) ;
#4038 = FACE_OUTER_BOUND ( 'NONE', #12818, .T. ) ;
#4039 = DIRECTION ( 'NONE',  ( 0.000000000000000000, 0.000000000000000000, -1.000000000000000000 ) ) ;
#4040 = AXIS2_PLACEMENT_3D ( 'NONE', #1502, #11325, #12788 ) ;
#4041 = CIRCLE ( 'NONE', #17739, 10.00000000000000000 ) ;
#4042 = CARTESIAN_POINT ( 'NONE',  ( -15.49999999999999822, -20.99999999999999645, 4.000000000000000000 ) ) ;
#4043 = CARTESIAN_POINT ( 'NONE',  ( 3.321934647848983957, -9.834888441627915867, 2.750161776669472591 ) ) ;
#4044 = CARTESIAN_POINT ( 'NONE',  ( -0.000000000000000000, 11.64110105645932691, 0.000000000000000000 ) ) ;
#4045 = EDGE_CURVE ( 'NONE', #3619, #7837, #12577, .T. ) ;
#4046 = CARTESIAN_POINT ( 'NONE',  ( 12.63806878948643231, -20.34002613093225520, 5.891296472647073124 ) ) ;
#4047 = DIRECTION ( 'NONE',  ( -1.000000000000000000, 0.000000000000000000, 0.000000000000000000 ) ) ;
#4048 = EDGE_CURVE ( 'NONE', #14054, #20705, #8197, .T. ) ;
#4049 = CARTESIAN_POINT ( 'NONE',  ( 11.69094141768317741, -22.74294823697955081, 4.171265325393542334 ) ) ;
#4050 = CARTESIAN_POINT ( 'NONE',  ( -12.62499999999998224, -20.25000000000006395, 4.416666666666681174 ) ) ;
#4051 = CARTESIAN_POINT ( 'NONE',  ( -7.097191417683176518, -22.46490103525075810, 4.479004561291653808 ) ) ;
#4052 = CARTESIAN_POINT ( 'NONE',  ( -9.815941417683177406, -20.26807450282663225, 5.303608408759377113 ) ) ;
#4053 = VERTEX_POINT ( 'NONE', #6309 ) ;
#4054 = CARTESIAN_POINT ( 'NONE',  ( 12.62562661273123332, -19.46835605706984040, 4.628101975944573176 ) ) ;
#4055 = CARTESIAN_POINT ( 'NONE',  ( -13.12529397354238192, 5.014845663890295846, 4.666666666666619889 ) ) ;
#4056 = ORIENTED_EDGE ( 'NONE', *, *, #20680, .T. ) ;
#4057 = AXIS2_PLACEMENT_3D ( 'NONE', #5691, #15608, #2761 ) ;
#4058 = CARTESIAN_POINT ( 'NONE',  ( -15.11404127825609223, 0.000000000000000000, 1.000000000000000000 ) ) ;
#4059 = DIRECTION ( 'NONE',  ( -0.000000000000000000, -0.000000000000000000, -1.000000000000000000 ) ) ;
#4060 = ORIENTED_EDGE ( 'NONE', *, *, #13780, .T. ) ;
#4061 = ORIENTED_EDGE ( 'NONE', *, *, #18921, .T. ) ;
#4062 = EDGE_CURVE ( 'NONE', #20665, #10724, #19190, .T. ) ;
#4063 = ORIENTED_EDGE ( 'NONE', *, *, #4119, .T. ) ;
#4064 = CARTESIAN_POINT ( 'NONE',  ( -4.999999999999998224, -2.500000000000047518, 9.999999999999998224 ) ) ;
#4065 = CARTESIAN_POINT ( 'NONE',  ( 13.00000000000000355, 7.806255641895631925E-15, 2.000000000000000000 ) ) ;
#4066 = CARTESIAN_POINT ( 'NONE',  ( -3.002445346198714837, -11.66215945560911749, 2.276826493710632171 ) ) ;
#4067 = LINE ( 'NONE', #4267, #12028 ) ;
#4068 = FACE_OUTER_BOUND ( 'NONE', #8866, .T. ) ;
#4069 = VECTOR ( 'NONE', #13961, 1000.000000000000000 ) ;
#4070 = LINE ( 'NONE', #12010, #4008 ) ;
#4071 = CARTESIAN_POINT ( 'NONE',  ( 11.87844141768317741, -24.50000000000000000, 3.449312527122335048 ) ) ;
#4072 = CARTESIAN_POINT ( 'NONE',  ( -12.64387510712649565, -19.29680709011273976, 5.506486987317513737 ) ) ;
#4073 = CARTESIAN_POINT ( 'NONE',  ( -9.628441417683177406, -19.49999999999998934, 3.550687472877664952 ) ) ;
#4074 = ORIENTED_EDGE ( 'NONE', *, *, #18619, .F. ) ;
#4075 = CARTESIAN_POINT ( 'NONE',  ( 12.34030858231679240, -22.67418626127525982, 5.270995438708342640 ) ) ;
#4076 = CARTESIAN_POINT ( 'NONE',  ( 0.000000000000000000, 4.999999999999999112, 1.000000000000000000 ) ) ;
#4077 = CARTESIAN_POINT ( 'NONE',  ( -13.86616162069444691, 3.803661845068127878, 6.738770894197415373 ) ) ;
#4078 = CARTESIAN_POINT ( 'NONE',  ( 12.24655858231679240, -21.94931252712234482, 5.250000000000000888 ) ) ;
#4079 = LINE ( 'NONE', #5648, #971 ) ;
#4080 = ORIENTED_EDGE ( 'NONE', *, *, #12578, .T. ) ;
#4081 = VERTEX_POINT ( 'NONE', #3177 ) ;
#4082 = CARTESIAN_POINT ( 'NONE',  ( 13.83544900551672185, 3.002674778589386140, 5.971513032956590195 ) ) ;
#4083 = CARTESIAN_POINT ( 'NONE',  ( 3.999999999999999112, -7.500000000000047073, 7.000000000000000000 ) ) ;
#4084 =( NAMED_UNIT ( * ) SI_UNIT ( $, .STERADIAN. ) SOLID_ANGLE_UNIT ( ) );
#4085 = ORIENTED_EDGE ( 'NONE', *, *, #19157, .F. ) ;
#4086 = AXIS2_PLACEMENT_3D ( 'NONE', #7917, #3418, #6662 ) ;
#4087 = EDGE_CURVE ( 'NONE', #10101, #19407, #9551, .T. ) ;
#4088 = FACE_OUTER_BOUND ( 'NONE', #16266, .T. ) ;
#4089 = DIRECTION ( 'NONE',  ( 0.000000000000000000, 1.000000000000000000, 0.000000000000000000 ) ) ;
#4090 = LINE ( 'NONE', #15065, #20007 ) ;
#4091 = CARTESIAN_POINT ( 'NONE',  ( 13.87467358130843387, 4.983515856073828409, 5.065827972856573602 ) ) ;
#4092 = DIRECTION ( 'NONE',  ( 1.000000000000000000, 0.000000000000000000, 0.000000000000000000 ) ) ;
#4093 = CARTESIAN_POINT ( 'NONE',  ( 3.528325504133930313, -10.14411005961392398, 2.079576065490765124 ) ) ;
#4094 = VECTOR ( 'NONE', #17098, 1000.000000000000000 ) ;
#4095 = DIRECTION ( 'NONE',  ( -0.000000000000000000, -0.000000000000000000, -1.000000000000000000 ) ) ;
#4096 = CARTESIAN_POINT ( 'NONE',  ( -13.12529397354238192, 5.014845663890295846, 4.333333333333382775 ) ) ;
#4097 = CARTESIAN_POINT ( 'NONE',  ( 10.84030858231679240, -22.67418626127525982, 5.270995438708342640 ) ) ;
#4098 = CARTESIAN_POINT ( 'NONE',  ( -13.86616162069444691, 3.803661845068127878, 6.738770894197415373 ) ) ;
#4099 = AXIS2_PLACEMENT_3D ( 'NONE', #14136, #17270, #11114 ) ;
#4100 = PLANE ( 'NONE',  #16718 ) ;
#4101 = CARTESIAN_POINT ( 'NONE',  ( 10.65280858231679240, -21.22443879296942626, 5.229004561291659137 ) ) ;
#4102 = CARTESIAN_POINT ( 'NONE',  ( 5.409691417683178294, -21.32581373872474373, 5.270995438708348857 ) ) ;
#4103 = CARTESIAN_POINT ( 'NONE',  ( -12.99655858231679417, -22.05068747287764452, 1.749999999999998446 ) ) ;
#4104 = VERTEX_POINT ( 'NONE', #17817 ) ;
#4105 = CARTESIAN_POINT ( 'NONE',  ( 12.67822638532683577, -18.31206754099172684, 6.277704579156187847 ) ) ;
#4106 = CARTESIAN_POINT ( 'NONE',  ( 12.62917185724685254, -19.28932120903463598, 4.753410794856941735 ) ) ;
#4107 = DIRECTION ( 'NONE',  ( 0.000000000000000000, -0.000000000000000000, 1.000000000000000000 ) ) ;
#4108 = VERTEX_POINT ( 'NONE', #7979 ) ;
#4109 = ORIENTED_EDGE ( 'NONE', *, *, #11312, .F. ) ;
#4110 = DIRECTION ( 'NONE',  ( 0.000000000000000000, -1.000000000000000000, 0.000000000000000000 ) ) ;
#4111 = VECTOR ( 'NONE', #8387, 1000.000000000000000 ) ;
#4112 = EDGE_CURVE ( 'NONE', #4793, #15521, #15923, .T. ) ;
#4113 = CARTESIAN_POINT ( 'NONE',  ( -12.64387510712649565, -19.29680709011273976, 5.506486987317513737 ) ) ;
#4114 = CARTESIAN_POINT ( 'NONE',  ( -7.626396343307448866, 0.000000000000000000, 0.000000000000000000 ) ) ;
#4115 = EDGE_CURVE ( 'NONE', #13899, #8944, #6425, .T. ) ;
#4116 = LINE ( 'NONE', #12474, #17071 ) ;
#4117 = CARTESIAN_POINT ( 'NONE',  ( 1.824488249492779879, -9.124319963227819130, 2.375058613629473570 ) ) ;
#4118 = DIRECTION ( 'NONE',  ( 1.000000000000000000, 0.000000000000000000, 0.000000000000000000 ) ) ;
#4119 = EDGE_CURVE ( 'NONE', #8041, #16594, #9859, .T. ) ;
#4120 = CYLINDRICAL_SURFACE ( 'NONE', #4057, 1.499999999999996891 ) ;
#4121 = CARTESIAN_POINT ( 'NONE',  ( -1.655860418491166941, -9.114909740826840689, 2.372641880528837621 ) ) ;
#4122 = CARTESIAN_POINT ( 'NONE',  ( -12.90280858231679595, -23.08622137881038938, 1.020995438708339309 ) ) ;
#4123 = CARTESIAN_POINT ( 'NONE',  ( -0.9854920305337621089, -9.114917468222230923, 1.622643865078341463 ) ) ;
#4124 = ORIENTED_EDGE ( 'NONE', *, *, #2849, .T. ) ;
#4125 = CARTESIAN_POINT ( 'NONE',  ( -13.80173896975277437, 2.050317972508536535, 5.200999963382010094 ) ) ;
#4126 = DIRECTION ( 'NONE',  ( 1.000000000000000000, 0.000000000000000000, 0.000000000000000000 ) ) ;
#4127 = CARTESIAN_POINT ( 'NONE',  ( 9.253441417683177406, -21.94931252712233061, 0.9999999999999978906 ) ) ;
#4128 = CARTESIAN_POINT ( 'NONE',  ( -8.315941417683177406, -21.32873467460645145, 4.242948236979555254 ) ) ;
#4129 = ORIENTED_EDGE ( 'NONE', *, *, #15235, .T. ) ;
#4130 = CARTESIAN_POINT ( 'NONE',  ( 13.39722611581222189, -19.12758115148224647, 5.495601574623241170 ) ) ;
#4131 = DIRECTION ( 'NONE',  ( -0.000000000000000000, -0.000000000000000000, -1.000000000000000000 ) ) ;
#4132 = ORIENTED_EDGE ( 'NONE', *, *, #12158, .F. ) ;
#4133 = ORIENTED_EDGE ( 'NONE', *, *, #11381, .F. ) ;
#4134 = LINE ( 'NONE', #5394, #11484 ) ;
#4135 = ORIENTED_EDGE ( 'NONE', *, *, #8761, .T. ) ;
#4136 = CARTESIAN_POINT ( 'NONE',  ( -13.83544900551672185, 3.002674778589386140, 5.971513032956590195 ) ) ;
#4137 = EDGE_CURVE ( 'NONE', #3725, #7631, #1600, .T. ) ;
#4138 = ORIENTED_EDGE ( 'NONE', *, *, #6597, .F. ) ;
#4139 = LINE ( 'NONE', #15320, #18012 ) ;
#4140 = CYLINDRICAL_SURFACE ( 'NONE', #4331, 10.00000000000000000 ) ;
#4141 =( BOUNDED_SURFACE ( )  B_SPLINE_SURFACE ( 3, 3, ( 
 ( #18451, #8924, #15293, #974, #13724, #9032, #20129, #5790, #10594, #16966, #2644, #15402, #7466, #13825, #20229, #5889, #4321, #9230, #18763, #10704, #7563, #20329, #5993, #12368, #4428, #10812, #17589, #1702, #14035, #20545, #7775, #25, #7968, #10910, #17486, #3264, #17698, #9639, #1392, #12878 ),
 ( #20639, #6296, #6516, #15912, #6197, #3371, #19180, #6412, #14138, #17272, #12777, #18965, #4619, #2954, #16025, #4833, #12565, #7871, #15601, #20445, #17384, #9334, #8085, #14449, #132, #11014, #19282, #3066, #18865, #4933, #11314, #11215, #1286, #3167, #7666, #15710, #4525, #6101, #9440, #15813 ),
 ( #12471, #1490, #14231, #12669, #19072, #14341, #4729, #11116, #9539, #1589, #11422, #824, #3954, #724, #17806, #5632, #12007, #7108, #11801, #921, #5430, #15149, #9750, #13569, #14553, #614, #16133, #10137, #7001, #13368, #13472, #19874, #225, #8186, #5529, #2182, #18191, #1800, #6613, #12983 ),
 ( #10342, #16712, #19771, #3856, #4066, #2280, #10234, #11900, #18291, #2389, #5045, #16822, #18403, #10453, #16600, #2486, #8670, #19386, #8879, #15247, #7309, #13671, #8780, #12116, #3758, #16509, #8565, #15040, #14934, #7208, #19972, #20079, #5745, #18508, #10866, #15457, #10651, #12523, #20595, #4577 ),
 ( #15662, #18818, #15559, #5847, #20499, #6155, #1241, #5941, #15765, #20284, #9285, #4168, #7726, #8978, #1141, #10549, #4266, #7519, #13883, #7615, #13983, #15352, #2591, #20392, #17025, #12315, #16919, #1034, #7420, #6054, #12216, #4482, #13782, #18918, #18712, #14090, #9184, #4377, #17334, #20187 ),
 ( #18604, #2704, #9087, #10760, #17130, #2809, #12422, #17231, #10963, #12620, #1447, #2910, #1346, #3017, #9393, #7825, #14188, #6246, #277, #5096, #17441, #3217, #11169, #3425, #11368, #14285, #181, #6669, #391, #13040, #4784, #16283, #19441, #1755, #9803, #8336, #16189, #17540, #11477, #1543 ),
 ( #9589, #20698, #1854, #1649, #8032, #6361, #17857, #8238, #15965, #11262, #6774, #14400, #4679, #83, #12830, #3526, #9902, #1954, #14714, #3120, #6471, #19232, #14602, #17756, #12731, #6565, #19025, #11072, #9494, #4883, #15865, #7921, #8141, #19132, #17642, #3317, #9698, #16085, #14503, #12928 ) ),
 .UNSPECIFIED., .T., .F., .F. ) 
 B_SPLINE_SURFACE_WITH_KNOTS ( ( 4, 3, 4 ),
 ( 4, 2, 2, 2, 2, 2, 2, 2, 2, 2, 2, 2, 2, 2, 2, 2, 2, 2, 2, 4 ),
 ( 0.000000000000000000, 0.5000000000000000000, 1.000000000000000000 ),
 ( 0.000000000000000000, 0.3100443560520446118, 0.4650665340780669177, 0.5425776230910780429, 0.5813331675975836887, 0.6007109398508364562, 0.6200887121040892236, 0.6309950902025724950, 0.6419014683010558775, 0.6637142244980225314, 0.7073397368919559502, 0.7509652492858893691, 0.7727780054828560230, 0.7836843835813394055, 0.7945907616798226769, 0.8074288390748337596, 0.8202669164698448423, 0.8459430712598670077, 0.8972953808399113385, 1.000000000000000000 ),
 .UNSPECIFIED. ) 
 GEOMETRIC_REPRESENTATION_ITEM ( )  RATIONAL_B_SPLINE_SURFACE ( (
 ( 1.000000000000000000, 1.000000000000000000, 1.000000000000000000, 1.000000000000000000, 1.000000000000000000, 1.000000000000000000, 1.000000000000000000, 1.000000000000000000, 1.000000000000000000, 1.000000000000000000, 1.000000000000000000, 1.000000000000000000, 1.000000000000000000, 1.000000000000000000, 1.000000000000000000, 1.000000000000000000, 1.000000000000000000, 1.000000000000000000, 1.000000000000000000, 1.000000000000000000, 1.000000000000000000, 1.000000000000000000, 1.000000000000000000, 1.000000000000000000, 1.000000000000000000, 1.000000000000000000, 1.000000000000000000, 1.000000000000000000, 1.000000000000000000, 1.000000000000000000, 1.000000000000000000, 1.000000000000000000, 1.000000000000000000, 1.000000000000000000, 1.000000000000000000, 1.000000000000000000, 1.000000000000000000, 1.000000000000000000, 1.000000000000000000, 1.000000000000000000),
 ( 0.3333333333333333703, 0.3333333333333333703, 0.3333333333333333703, 0.3333333333333333703, 0.3333333333333333703, 0.3333333333333333703, 0.3333333333333333703, 0.3333333333333333703, 0.3333333333333333703, 0.3333333333333333703, 0.3333333333333333703, 0.3333333333333333703, 0.3333333333333333703, 0.3333333333333333703, 0.3333333333333333703, 0.3333333333333333703, 0.3333333333333333703, 0.3333333333333333703, 0.3333333333333333703, 0.3333333333333333703, 0.3333333333333333703, 0.3333333333333333703, 0.3333333333333333703, 0.3333333333333333703, 0.3333333333333333703, 0.3333333333333333703, 0.3333333333333333703, 0.3333333333333333703, 0.3333333333333333703, 0.3333333333333333703, 0.3333333333333333703, 0.3333333333333333703, 0.3333333333333333703, 0.3333333333333333703, 0.3333333333333333703, 0.3333333333333333703, 0.3333333333333333703, 0.3333333333333333703, 0.3333333333333333703, 0.3333333333333333703),
 ( 0.3333333333333333703, 0.3333333333333333703, 0.3333333333333333703, 0.3333333333333333703, 0.3333333333333333703, 0.3333333333333333703, 0.3333333333333333703, 0.3333333333333333703, 0.3333333333333333703, 0.3333333333333333703, 0.3333333333333333703, 0.3333333333333333703, 0.3333333333333333703, 0.3333333333333333703, 0.3333333333333333703, 0.3333333333333333703, 0.3333333333333333703, 0.3333333333333333703, 0.3333333333333333703, 0.3333333333333333703, 0.3333333333333333703, 0.3333333333333333703, 0.3333333333333333703, 0.3333333333333333703, 0.3333333333333333703, 0.3333333333333333703, 0.3333333333333333703, 0.3333333333333333703, 0.3333333333333333703, 0.3333333333333333703, 0.3333333333333333703, 0.3333333333333333703, 0.3333333333333333703, 0.3333333333333333703, 0.3333333333333333703, 0.3333333333333333703, 0.3333333333333333703, 0.3333333333333333703, 0.3333333333333333703, 0.3333333333333333703),
 ( 1.000000000000000000, 1.000000000000000000, 1.000000000000000000, 1.000000000000000000, 1.000000000000000000, 1.000000000000000000, 1.000000000000000000, 1.000000000000000000, 1.000000000000000000, 1.000000000000000000, 1.000000000000000000, 1.000000000000000000, 1.000000000000000000, 1.000000000000000000, 1.000000000000000000, 1.000000000000000000, 1.000000000000000000, 1.000000000000000000, 1.000000000000000000, 1.000000000000000000, 1.000000000000000000, 1.000000000000000000, 1.000000000000000000, 1.000000000000000000, 1.000000000000000000, 1.000000000000000000, 1.000000000000000000, 1.000000000000000000, 1.000000000000000000, 1.000000000000000000, 1.000000000000000000, 1.000000000000000000, 1.000000000000000000, 1.000000000000000000, 1.000000000000000000, 1.000000000000000000, 1.000000000000000000, 1.000000000000000000, 1.000000000000000000, 1.000000000000000000),
 ( 0.3333333333333333703, 0.3333333333333333703, 0.3333333333333333703, 0.3333333333333333703, 0.3333333333333333703, 0.3333333333333333703, 0.3333333333333333703, 0.3333333333333333703, 0.3333333333333333703, 0.3333333333333333703, 0.3333333333333333703, 0.3333333333333333703, 0.3333333333333333703, 0.3333333333333333703, 0.3333333333333333703, 0.3333333333333333703, 0.3333333333333333703, 0.3333333333333333703, 0.3333333333333333703, 0.3333333333333333703, 0.3333333333333333703, 0.3333333333333333703, 0.3333333333333333703, 0.3333333333333333703, 0.3333333333333333703, 0.3333333333333333703, 0.3333333333333333703, 0.3333333333333333703, 0.3333333333333333703, 0.3333333333333333703, 0.3333333333333333703, 0.3333333333333333703, 0.3333333333333333703, 0.3333333333333333703, 0.3333333333333333703, 0.3333333333333333703, 0.3333333333333333703, 0.3333333333333333703, 0.3333333333333333703, 0.3333333333333333703),
 ( 0.3333333333333333703, 0.3333333333333333703, 0.3333333333333333703, 0.3333333333333333703, 0.3333333333333333703, 0.3333333333333333703, 0.3333333333333333703, 0.3333333333333333703, 0.3333333333333333703, 0.3333333333333333703, 0.3333333333333333703, 0.3333333333333333703, 0.3333333333333333703, 0.3333333333333333703, 0.3333333333333333703, 0.3333333333333333703, 0.3333333333333333703, 0.3333333333333333703, 0.3333333333333333703, 0.3333333333333333703, 0.3333333333333333703, 0.3333333333333333703, 0.3333333333333333703, 0.3333333333333333703, 0.3333333333333333703, 0.3333333333333333703, 0.3333333333333333703, 0.3333333333333333703, 0.3333333333333333703, 0.3333333333333333703, 0.3333333333333333703, 0.3333333333333333703, 0.3333333333333333703, 0.3333333333333333703, 0.3333333333333333703, 0.3333333333333333703, 0.3333333333333333703, 0.3333333333333333703, 0.3333333333333333703, 0.3333333333333333703),
 ( 1.000000000000000000, 1.000000000000000000, 1.000000000000000000, 1.000000000000000000, 1.000000000000000000, 1.000000000000000000, 1.000000000000000000, 1.000000000000000000, 1.000000000000000000, 1.000000000000000000, 1.000000000000000000, 1.000000000000000000, 1.000000000000000000, 1.000000000000000000, 1.000000000000000000, 1.000000000000000000, 1.000000000000000000, 1.000000000000000000, 1.000000000000000000, 1.000000000000000000, 1.000000000000000000, 1.000000000000000000, 1.000000000000000000, 1.000000000000000000, 1.000000000000000000, 1.000000000000000000, 1.000000000000000000, 1.000000000000000000, 1.000000000000000000, 1.000000000000000000, 1.000000000000000000, 1.000000000000000000, 1.000000000000000000, 1.000000000000000000, 1.000000000000000000, 1.000000000000000000, 1.000000000000000000, 1.000000000000000000, 1.000000000000000000, 1.000000000000000000) ) ) 
 REPRESENTATION_ITEM ( '' )  SURFACE ( )  );
#4142 = DIRECTION ( 'NONE',  ( 0.000000000000000000, 0.000000000000000000, 1.000000000000000000 ) ) ;
#4143 = CARTESIAN_POINT ( 'NONE',  ( 3.882031223148668886, -13.81156101447257889, 3.771450735391772557 ) ) ;
#4144 = CARTESIAN_POINT ( 'NONE',  ( -4.000000000000000000, -8.500000000000000000, 1.000000000000000000 ) ) ;
#4145 = CARTESIAN_POINT ( 'NONE',  ( 13.90394305879618386, 5.711624469205903942, 5.287712306078340418 ) ) ;
#4146 = CARTESIAN_POINT ( 'NONE',  ( -13.67791111847408025, 4.999999999999999112, 1.000000000000000000 ) ) ;
#4147 = CARTESIAN_POINT ( 'NONE',  ( 0.000000000000000000, 0.000000000000000000, 4.000000000000000000 ) ) ;
#4148 = LINE ( 'NONE', #10742, #12705 ) ;
#4149 = CARTESIAN_POINT ( 'NONE',  ( 12.53469141768317741, -20.97900456129164581, 3.136473910504570917 ) ) ;
#4150 = CARTESIAN_POINT ( 'NONE',  ( -12.62499999998404121, -20.24999999996810729, 2.793053905886972998 ) ) ;
#4151 = EDGE_CURVE ( 'NONE', #14709, #13797, #4844, .T. ) ;
#4152 = CARTESIAN_POINT ( 'NONE',  ( -13.37155858231679595, -20.99999999999999645, 3.449312527122348371 ) ) ;
#4153 = CARTESIAN_POINT ( 'NONE',  ( -12.44094141768317741, -20.19639159124061933, 1.768074502826635586 ) ) ;
#4154 = VERTEX_POINT ( 'NONE', #142 ) ;
#4155 = CARTESIAN_POINT ( 'NONE',  ( 12.63238774201960268, -19.12691902800888499, 4.760115940007608515 ) ) ;
#4156 = CARTESIAN_POINT ( 'NONE',  ( -13.00900269284621302, -0.8578640112522492034, 5.903024842915844062 ) ) ;
#4157 = EDGE_LOOP ( 'NONE', ( #19044, #9687, #1133, #18155 ) ) ;
#4158 = DIRECTION ( 'NONE',  ( -0.000000000000000000, -0.000000000000000000, -1.000000000000000000 ) ) ;
#4159 = CARTESIAN_POINT ( 'NONE',  ( 3.499999999999998668, -24.49999999999999289, 1.000000000000000000 ) ) ;
#4160 = ORIENTED_EDGE ( 'NONE', *, *, #520, .F. ) ;
#4161 = EDGE_LOOP ( 'NONE', ( #2902, #3005, #20613, #16756 ) ) ;
#4162 = ADVANCED_FACE ( 'NONE', ( #12889 ), #8294, .T. ) ;
#4163 = EDGE_CURVE ( 'NONE', #6020, #19964, #19501, .T. ) ;
#4164 = ORIENTED_EDGE ( 'NONE', *, *, #17052, .F. ) ;
#4165 = CARTESIAN_POINT ( 'NONE',  ( -17.94064177244175795, 11.64110105645932691, 10.00000000000000000 ) ) ;
#4166 = DIRECTION ( 'NONE',  ( -0.000000000000000000, -0.000000000000000000, -1.000000000000000000 ) ) ;
#4167 = EDGE_CURVE ( 'NONE', #9694, #16571, #8406, .T. ) ;
#4168 = CARTESIAN_POINT ( 'NONE',  ( -2.067263844777544435, -10.27417889452513933, 1.727750375171331676 ) ) ;
#4169 = DIRECTION ( 'NONE',  ( 0.000000000000000000, 1.000000000000000000, 0.000000000000000000 ) ) ;
#4170 = DIRECTION ( 'NONE',  ( -1.000000000000000000, 0.000000000000000000, -0.000000000000000000 ) ) ;
#4171 = CARTESIAN_POINT ( 'NONE',  ( 25.04469207716615031, 0.000000000000000000, 1.000000000000000000 ) ) ;
#4172 = CARTESIAN_POINT ( 'NONE',  ( 4.717959273841179524, -21.63341328858655999, 5.993595146365859883 ) ) ;
#4173 = CARTESIAN_POINT ( 'NONE',  ( -13.11017182064853159, 4.251176942750957366, 5.979809059808775196 ) ) ;
#4174 = ADVANCED_FACE ( 'NONE', ( #16342 ), #2017, .T. ) ;
#4175 = CARTESIAN_POINT ( 'NONE',  ( -5.784691417683178294, -24.52099543870834708, 4.484846433055073689 ) ) ;
#4176 = ORIENTED_EDGE ( 'NONE', *, *, #16737, .T. ) ;
#4177 = CARTESIAN_POINT ( 'NONE',  ( 12.62155858231679417, -23.74999999999999645, 3.550687472877651629 ) ) ;
#4178 = DIRECTION ( 'NONE',  ( 0.000000000000000000, 1.000000000000000000, 0.000000000000000000 ) ) ;
#4179 = CARTESIAN_POINT ( 'NONE',  ( -13.82120031190154208, 1.533115751011936867, 6.689942769197355865 ) ) ;
#4180 = CARTESIAN_POINT ( 'NONE',  ( 4.717959273841179524, -21.82295283170803302, 4.493595146365858994 ) ) ;
#4181 = LINE ( 'NONE', #10357, #11656 ) ;
#4182 = ORIENTED_EDGE ( 'NONE', *, *, #5534, .F. ) ;
#4183 = ORIENTED_EDGE ( 'NONE', *, *, #3651, .T. ) ;
#4184 = CARTESIAN_POINT ( 'NONE',  ( 13.39782821820594627, -19.84717498059871943, 6.143582220458365661 ) ) ;
#4185 = LINE ( 'NONE', #15575, #2909 ) ;
#4186 = SHAPE_REPRESENTATION_RELATIONSHIP ( 'NONE' , 'NONE' ,  #19662, #4314 ) ;
#4187 = EDGE_LOOP ( 'NONE', ( #15880, #14734, #14736, #13079 ) ) ;
#4188 = CARTESIAN_POINT ( 'NONE',  ( 30.00000000000000000, 10.00000000000000000, 1.000000000000000000 ) ) ;
#4189 = CIRCLE ( 'NONE', #18271, 1.499999999999996225 ) ;
#4190 = ORIENTED_EDGE ( 'NONE', *, *, #6734, .F. ) ;
#4191 = CARTESIAN_POINT ( 'NONE',  ( -12.80905858231679417, -23.27327832286945153, 2.298404588716537411 ) ) ;
#4192 = CARTESIAN_POINT ( 'NONE',  ( 13.86693669322925260, 4.592803008081209448, 5.801483467520450077 ) ) ;
#4193 = AXIS2_PLACEMENT_3D ( 'NONE', #1828, #1620, #12703 ) ;
#4194 = DIRECTION ( 'NONE',  ( 0.000000000000000000, 0.000000000000000000, -1.000000000000000000 ) ) ;
#4195 = CARTESIAN_POINT ( 'NONE',  ( 2.787023586469211001, -10.13267000451481614, 1.884023048047904103 ) ) ;
#4196 = CARTESIAN_POINT ( 'NONE',  ( 9.000000000000000000, -9.999999999999991118, 2.500000000000000000 ) ) ;
#4197 = CARTESIAN_POINT ( 'NONE',  ( -13.37500000000002132, -19.49999999999450040, 3.833333333368183382 ) ) ;
#4198 = CARTESIAN_POINT ( 'NONE',  ( 12.15280858231679595, -21.22443879296942626, 5.229004561291659137 ) ) ;
#4199 = CARTESIAN_POINT ( 'NONE',  ( -13.56222317325195093, -11.54522975075300728, 6.408692769197242178 ) ) ;
#4200 = EDGE_CURVE ( 'NONE', #19645, #10336, #7057, .T. ) ;
#4201 = CARTESIAN_POINT ( 'NONE',  ( -15.49999999999999822, -22.99999999999999289, 4.000000000000000000 ) ) ;
#4202 = CARTESIAN_POINT ( 'NONE',  ( 10.37155858231679417, -20.24999999999999289, 3.449312527122348371 ) ) ;
#4203 = CARTESIAN_POINT ( 'NONE',  ( 10.56594141768317741, -22.67126532539353789, 2.757051763020445634 ) ) ;
#4204 = CARTESIAN_POINT ( 'NONE',  ( -8.777808582316792396, -20.27099543870833642, 2.724438792969431589 ) ) ;
#4205 = ORIENTED_EDGE ( 'NONE', *, *, #4910, .F. ) ;
#4206 = CARTESIAN_POINT ( 'NONE',  ( 13.09073190589589331, 4.019461247742575516, 5.257453802652931607 ) ) ;
#4207 = FACE_OUTER_BOUND ( 'NONE', #8278, .T. ) ;
#4208 = ORIENTED_EDGE ( 'NONE', *, *, #13574, .F. ) ;
#4209 = VERTEX_POINT ( 'NONE', #1928 ) ;
#4210 = LINE ( 'NONE', #15400, #8450 ) ;
#4211 = PRODUCT_RELATED_PRODUCT_CATEGORY ( 'part', '', ( #6339 ) ) ;
#4212 = VECTOR ( 'NONE', #13653, 1000.000000000000000 ) ;
#4213 = CARTESIAN_POINT ( 'NONE',  ( -13.02818618459764188, 0.1109023222084986743, 5.923858176248589125 ) ) ;
#4214 = CARTESIAN_POINT ( 'NONE',  ( -9.000000000000000000, -9.999999999999992895, 2.500000000000000000 ) ) ;
#4215 = CARTESIAN_POINT ( 'NONE',  ( -13.86693669322925260, 4.592803008081209448, 5.801483467520450077 ) ) ;
#4216 = DIRECTION ( 'NONE',  ( 1.000000000000000000, 0.000000000000000000, 0.000000000000000000 ) ) ;
#4217 = CARTESIAN_POINT ( 'NONE',  ( -12.62499999999998579, -20.24999999999999289, 3.666666666666653640 ) ) ;
#4218 = LINE ( 'NONE', #7470, #8160 ) ;
#4219 = DIRECTION ( 'NONE',  ( 0.000000000000000000, 0.000000000000000000, 1.000000000000000000 ) ) ;
#4220 = DIRECTION ( 'NONE',  ( 0.000000000000000000, 0.000000000000000000, 1.000000000000000000 ) ) ;
#4221 = CARTESIAN_POINT ( 'NONE',  ( -11.02780858231679595, -24.47900456129166358, 4.586221378810390270 ) ) ;
#4222 = CARTESIAN_POINT ( 'NONE',  ( -2.722060606927515725, -8.660968749821154944, 1.698675748411476283 ) ) ;
#4223 = VERTEX_POINT ( 'NONE', #3500 ) ;
#4224 = CARTESIAN_POINT ( 'NONE',  ( -13.37499999999998579, -20.24999999999999289, 3.146526952850934755 ) ) ;
#4225 = LINE ( 'NONE', #17286, #4372 ) ;
#4226 = EDGE_CURVE ( 'NONE', #18281, #11254, #776, .T. ) ;
#4227 = CARTESIAN_POINT ( 'NONE',  ( 10.75344141768317741, -21.94931252712233061, 0.9999999999999978906 ) ) ;
#4228 = CARTESIAN_POINT ( 'NONE',  ( -9.159691417683175629, -22.36352608949543352, 2.479004561291652031 ) ) ;
#4229 = ORIENTED_EDGE ( 'NONE', *, *, #13976, .F. ) ;
#4230 = CARTESIAN_POINT ( 'NONE',  ( 13.37499999999998224, -20.24999999999998934, 4.291666666666698937 ) ) ;
#4231 = DIRECTION ( 'NONE',  ( 0.000000000000000000, 0.000000000000000000, 1.000000000000000000 ) ) ;
#4232 = ORIENTED_EDGE ( 'NONE', *, *, #7719, .F. ) ;
#4233 = VERTEX_POINT ( 'NONE', #7161 ) ;
#4234 = CARTESIAN_POINT ( 'NONE',  ( 4.000000000000000000, -8.500000000000000000, 1.000000000000000000 ) ) ;
#4235 = ORIENTED_EDGE ( 'NONE', *, *, #4541, .F. ) ;
#4236 = CARTESIAN_POINT ( 'NONE',  ( -13.87470602645761986, 4.985154336109792972, 4.833333333333344584 ) ) ;
#4237 = EDGE_CURVE ( 'NONE', #11568, #16197, #5584, .T. ) ;
#4238 = EDGE_CURVE ( 'NONE', #9082, #12662, #14990, .T. ) ;
#4239 = DIRECTION ( 'NONE',  ( 0.000000000000000000, 0.000000000000000000, 1.000000000000000000 ) ) ;
#4240 = AXIS2_PLACEMENT_3D ( 'NONE', #2331, #13615, #10281 ) ;
#4241 = ORIENTED_EDGE ( 'NONE', *, *, #3472, .F. ) ;
#4242 = LINE ( 'NONE', #6021, #16007 ) ;
#4243 = CARTESIAN_POINT ( 'NONE',  ( -14.49999999999998579, -18.49999999999999645, 4.000000000000000000 ) ) ;
#4244 = DIRECTION ( 'NONE',  ( -0.000000000000000000, -0.8660254037844364872, -0.5000000000000036637 ) ) ;
#4245 = CARTESIAN_POINT ( 'NONE',  ( 3.607313482701580476, -10.70492285834919244, 2.223603995567122293 ) ) ;
#4246 = DIRECTION ( 'NONE',  ( -0.000000000000000000, 0.000000000000000000, -1.000000000000000000 ) ) ;
#4247 = DIRECTION ( 'NONE',  ( 1.000000000000000000, 0.000000000000000000, 0.000000000000000000 ) ) ;
#4248 = DIRECTION ( 'NONE',  ( -1.000000000000000000, 0.000000000000000000, 0.000000000000000000 ) ) ;
#4249 = CARTESIAN_POINT ( 'NONE',  ( 13.12529397354238192, 5.014845663890295846, 3.666666666666500873 ) ) ;
#4250 = CARTESIAN_POINT ( 'NONE',  ( 5.315941417683176518, -20.79840458871654363, 4.773278322869464851 ) ) ;
#4251 = LINE ( 'NONE', #15133, #4212 ) ;
#4252 = CARTESIAN_POINT ( 'NONE',  ( -10.84030858231679595, -22.36352608949544418, 4.520995438708343528 ) ) ;
#4253 = ADVANCED_FACE ( 'NONE', ( #18145 ), #16360, .T. ) ;
#4254 = CARTESIAN_POINT ( 'NONE',  ( -9.628441417683177406, -19.49999999999998934, 3.550687472877664952 ) ) ;
#4255 = ORIENTED_EDGE ( 'NONE', *, *, #9260, .T. ) ;
#4256 = CARTESIAN_POINT ( 'NONE',  ( 12.62499999999998224, -19.49999999999998934, 4.166666666666637653 ) ) ;
#4257 = CARTESIAN_POINT ( 'NONE',  ( -13.12270769621861355, 4.884238659038159902, 5.513847264053151065 ) ) ;
#4258 = ORIENTED_EDGE ( 'NONE', *, *, #821, .T. ) ;
#4259 = CARTESIAN_POINT ( 'NONE',  ( -11.99999999999999822, -18.50000000000000355, 1.000000000000000000 ) ) ;
#4260 = CARTESIAN_POINT ( 'NONE',  ( 0.000000000000000000, 11.64110105645932691, 10.00000000000000000 ) ) ;
#4261 = ORIENTED_EDGE ( 'NONE', *, *, #12949, .T. ) ;
#4262 = CARTESIAN_POINT ( 'NONE',  ( 2.109407804498405703, -9.207748739546751438, 2.396484790045401603 ) ) ;
#4263 = ORIENTED_EDGE ( 'NONE', *, *, #16645, .T. ) ;
#4264 = DIRECTION ( 'NONE',  ( 0.000000000000000000, 1.000000000000000000, 0.000000000000000000 ) ) ;
#4265 = CARTESIAN_POINT ( 'NONE',  ( 3.747260319564023501, 0.000000000000000000, 1.000000000000000000 ) ) ;
#4266 = CARTESIAN_POINT ( 'NONE',  ( -2.041623931606483033, -10.12028065167953272, 1.688226231982305370 ) ) ;
#4267 = CARTESIAN_POINT ( 'NONE',  ( 1.811130159782011528, 4.999999999999999112, 1.000000000000000000 ) ) ;
#4268 = LINE ( 'NONE', #10868, #1291 ) ;
#4269 = CARTESIAN_POINT ( 'NONE',  ( -20.00000000000000000, -6.000000000000000000, 2.000000000000000000 ) ) ;
#4270 = CARTESIAN_POINT ( 'NONE',  ( 6.996558582316795949, -22.05068747287764452, 0.9999999999999978906 ) ) ;
#4271 = CARTESIAN_POINT ( 'NONE',  ( -12.64131715375063258, -19.42598373559290792, 5.491151580003103660 ) ) ;
#4272 = VECTOR ( 'NONE', #16203, 1000.000000000000000 ) ;
#4273 = CARTESIAN_POINT ( 'NONE',  ( -9.909691417683179182, -21.32581373872474373, 5.270995438708348857 ) ) ;
#4274 = EDGE_CURVE ( 'NONE', #6051, #19095, #18037, .T. ) ;
#4275 = EDGE_LOOP ( 'NONE', ( #7845, #2978, #8345, #16987 ) ) ;
#4276 = EDGE_CURVE ( 'NONE', #20415, #7096, #3810, .T. ) ;
#4277 = DIRECTION ( 'NONE',  ( -0.000000000000000000, -0.000000000000000000, -1.000000000000000000 ) ) ;
#4278 = LINE ( 'NONE', #15468, #9418 ) ;
#4279 = CARTESIAN_POINT ( 'NONE',  ( -13.40995420747273670, -19.23481252262645924, 6.243328185864100988 ) ) ;
#4280 = CARTESIAN_POINT ( 'NONE',  ( 10.46530858231679417, -20.22900456129164937, 4.174186261275266929 ) ) ;
#4281 = DIRECTION ( 'NONE',  ( -3.469446951953619119E-16, -1.000000000000000000, 0.000000000000000000 ) ) ;
#4282 = ORIENTED_EDGE ( 'NONE', *, *, #13693, .T. ) ;
#4283 = ORIENTED_EDGE ( 'NONE', *, *, #9109, .T. ) ;
#4284 = CARTESIAN_POINT ( 'NONE',  ( 13.41355111217617413, -19.05316883510194614, 6.247234435864091218 ) ) ;
#4285 = CARTESIAN_POINT ( 'NONE',  ( -15.49999999999998224, -17.49999999999999645, 1.000000000000000000 ) ) ;
#4286 = PRESENTATION_STYLE_ASSIGNMENT (( #12442 ) ) ;
#4287 = ORIENTED_EDGE ( 'NONE', *, *, #7398, .F. ) ;
#4288 = CIRCLE ( 'NONE', #12301, 1.000000000000002665 ) ;
#4289 = CARTESIAN_POINT ( 'NONE',  ( 15.50000000000000178, -23.00000000000000711, 4.000000000000000000 ) ) ;
#4290 = AXIS2_PLACEMENT_3D ( 'NONE', #3733, #2160, #13960 ) ;
#4291 = VERTEX_POINT ( 'NONE', #5481 ) ;
#4292 = EDGE_CURVE ( 'NONE', #17482, #2580, #13422, .T. ) ;
#4293 = CARTESIAN_POINT ( 'NONE',  ( -8.402808582316794173, -22.77556120703056308, 1.770995438708339975 ) ) ;
#4294 = CARTESIAN_POINT ( 'NONE',  ( 13.87367531042247748, 4.933103176334663331, 5.324010972534209074 ) ) ;
#4295 = CARTESIAN_POINT ( 'NONE',  ( 0.000000000000000000, 4.999999999999999112, 1.000000000000000000 ) ) ;
#4296 = CARTESIAN_POINT ( 'NONE',  ( 3.342893013439646843, -9.383962644129466568, 1.884355023724047173 ) ) ;
#4297 = CARTESIAN_POINT ( 'NONE',  ( 30.00000000000000000, 10.00000000000000000, 0.000000000000000000 ) ) ;
#4298 = CARTESIAN_POINT ( 'NONE',  ( -13.08919463935856697, 3.941829287606363863, 5.256209690007596080 ) ) ;
#4299 = AXIS2_PLACEMENT_3D ( 'NONE', #10111, #10211, #16578 ) ;
#4300 = CARTESIAN_POINT ( 'NONE',  ( 14.50000000000000000, -20.99999999999998934, 4.000000000000000000 ) ) ;
#4301 = CARTESIAN_POINT ( 'NONE',  ( -13.84997554952896515, 2.986265251207539606, 6.721192769197450012 ) ) ;
#4302 = EDGE_CURVE ( 'NONE', #4697, #7456, #5269, .T. ) ;
#4303 = VECTOR ( 'NONE', #1931, 1000.000000000000000 ) ;
#4304 = EDGE_CURVE ( 'NONE', #5740, #15982, #14687, .T. ) ;
#4305 = DIRECTION ( 'NONE',  ( 0.000000000000000000, -0.8660254037844364872, -0.5000000000000036637 ) ) ;
#4306 = CARTESIAN_POINT ( 'NONE',  ( 9.996558582316794173, -22.05068747287764452, 1.749999999999998446 ) ) ;
#4307 = CARTESIAN_POINT ( 'NONE',  ( 4.472191417683177406, -23.72900456129165292, 2.724438792969417822 ) ) ;
#4308 = CARTESIAN_POINT ( 'NONE',  ( -5.684058582316794173, -20.79840458871652942, 2.226721677130544030 ) ) ;
#4309 = ORIENTED_EDGE ( 'NONE', *, *, #16551, .T. ) ;
#4310 = CARTESIAN_POINT ( 'NONE',  ( 13.09533517714100093, 4.251926445620864747, 5.084080158857392284 ) ) ;
#4311 = DIRECTION ( 'NONE',  ( 0.000000000000000000, 0.000000000000000000, -1.000000000000000000 ) ) ;
#4312 = ORIENTED_EDGE ( 'NONE', *, *, #8911, .T. ) ;
#4313 = ORIENTED_EDGE ( 'NONE', *, *, #16286, .F. ) ;
#4314 = ADVANCED_BREP_SHAPE_REPRESENTATION ( '', ( #18044, #18039 ), #5348 ) ;
#4315 = DIRECTION ( 'NONE',  ( -0.000000000000000000, -0.000000000000000000, -1.000000000000000000 ) ) ;
#4316 = VECTOR ( 'NONE', #7495, 1000.000000000000000 ) ;
#4317 = EDGE_CURVE ( 'NONE', #12726, #9432, #18246, .T. ) ;
#4318 = CARTESIAN_POINT ( 'NONE',  ( -12.62499999999998224, -20.24999999999991829, 4.333333333333343695 ) ) ;
#4319 = VECTOR ( 'NONE', #11914, 1000.000000000000000 ) ;
#4320 = AXIS2_PLACEMENT_3D ( 'NONE', #10523, #10620, #8947 ) ;
#4321 = CARTESIAN_POINT ( 'NONE',  ( -2.559937518207947793, -9.746075135043517079, 2.534737762559237773 ) ) ;
#4322 = CARTESIAN_POINT ( 'NONE',  ( -13.84863765609603625, 3.668701632846259830, 5.985835949623216301 ) ) ;
#4323 = CARTESIAN_POINT ( 'NONE',  ( 0.000000000000000000, 4.999999999999999112, 1.000000000000000000 ) ) ;
#4324 = DIRECTION ( 'NONE',  ( 0.000000000000000000, 1.000000000000000000, 0.000000000000000000 ) ) ;
#4325 = LINE ( 'NONE', #17081, #3688 ) ;
#4326 = DIRECTION ( 'NONE',  ( -1.000000000000000000, 0.000000000000000000, 0.000000000000000000 ) ) ;
#4327 = DIRECTION ( 'NONE',  ( 0.000000000000000000, -1.000000000000000000, 0.000000000000000000 ) ) ;
#4328 = CARTESIAN_POINT ( 'NONE',  ( -10.46530858231679595, -19.47900456129164937, 4.484846433055089676 ) ) ;
#4329 = CARTESIAN_POINT ( 'NONE',  ( -1.548630333695928396, -9.114917468222230923, 1.622643865078341463 ) ) ;
#4330 = VERTEX_POINT ( 'NONE', #366 ) ;
#4331 = AXIS2_PLACEMENT_3D ( 'NONE', #16893, #8948, #20157 ) ;
#4332 = CARTESIAN_POINT ( 'NONE',  ( -13.37883250981221472, -20.05645825448334563, 5.102688967256983510 ) ) ;
#4333 = CARTESIAN_POINT ( 'NONE',  ( 26.04469207716615031, 4.999999999999999112, 1.000000000000000000 ) ) ;
#4334 = CARTESIAN_POINT ( 'NONE',  ( 11.22219141768317741, -19.52099543870834353, 4.586221378810406257 ) ) ;
#4335 = CARTESIAN_POINT ( 'NONE',  ( -7.378441417683177406, -22.99999999999999645, 3.449312527122335048 ) ) ;
#4336 = AXIS2_PLACEMENT_3D ( 'NONE', #20659, #19094, #14469 ) ;
#4337 = VERTEX_POINT ( 'NONE', #3909 ) ;
#4338 = CARTESIAN_POINT ( 'NONE',  ( 13.41355111217617413, -19.05316883510194614, 6.247234435864091218 ) ) ;
#4339 = FACE_OUTER_BOUND ( 'NONE', #8467, .T. ) ;
#4340 = ORIENTED_EDGE ( 'NONE', *, *, #7759, .F. ) ;
#4341 = ORIENTED_EDGE ( 'NONE', *, *, #7234, .T. ) ;
#4342 = LINE ( 'NONE', #8179, #4094 ) ;
#4343 = CIRCLE ( 'NONE', #15365, 0.3749999999999997224 ) ;
#4344 = EDGE_LOOP ( 'NONE', ( #16836, #12333, #7819, #140 ) ) ;
#4345 = CARTESIAN_POINT ( 'NONE',  ( -9.999999999999996447, -34.99999999999999289, 0.000000000000000000 ) ) ;
#4346 = CARTESIAN_POINT ( 'NONE',  ( 2.109407804498405703, -9.207748739546751438, 2.396484790045401603 ) ) ;
#4347 = ORIENTED_EDGE ( 'NONE', *, *, #10396, .F. ) ;
#4348 = DIRECTION ( 'NONE',  ( 1.156482317317871331E-15, -1.000000000000000000, 0.000000000000000000 ) ) ;
#4349 = CARTESIAN_POINT ( 'NONE',  ( -20.00000000000000000, -6.000000000000000000, 2.000000000000000000 ) ) ;
#4350 = EDGE_CURVE ( 'NONE', #20018, #5573, #19613, .T. ) ;
#4351 = CARTESIAN_POINT ( 'NONE',  ( 15.00000000000001421, -17.49999999999999645, 4.000000000000000000 ) ) ;
#4352 = CARTESIAN_POINT ( 'NONE',  ( 1.960495238260606010, -8.383787449798761671, 1.627490053312942164 ) ) ;
#4353 = CARTESIAN_POINT ( 'NONE',  ( -14.99999999999998579, -18.49999999999999645, 4.000000000000000000 ) ) ;
#4354 = CARTESIAN_POINT ( 'NONE',  ( 13.09892531043291086, 3.683228176858501790, 6.000681092915118420 ) ) ;
#4355 = VECTOR ( 'NONE', #2302, 1000.000000000000000 ) ;
#4356 = LINE ( 'NONE', #18690, #15295 ) ;
#4357 = PLANE ( 'NONE',  #6374 ) ;
#4358 = DIRECTION ( 'NONE',  ( 1.000000000000000000, 0.000000000000000000, 0.000000000000000000 ) ) ;
#4359 = CARTESIAN_POINT ( 'NONE',  ( 7.659691417683177406, -22.36352608949543352, 2.479004561291652031 ) ) ;
#4360 = CARTESIAN_POINT ( 'NONE',  ( -13.10372118337080849, 3.925419760224517329, 6.005889426248455010 ) ) ;
#4361 = CARTESIAN_POINT ( 'NONE',  ( -10.46530858231679595, -20.97900456129165647, 3.863526089495444626 ) ) ;
#4362 = VECTOR ( 'NONE', #18035, 1000.000000000000000 ) ;
#4363 = CARTESIAN_POINT ( 'NONE',  ( -10.47219141768317741, -24.47900456129165292, 2.413778621189595963 ) ) ;
#4364 = ORIENTED_EDGE ( 'NONE', *, *, #949, .T. ) ;
#4365 = CARTESIAN_POINT ( 'NONE',  ( 13.37500751150753864, -19.49962066887028556, 4.515663405036051792 ) ) ;
#4366 = CARTESIAN_POINT ( 'NONE',  ( -12.65410809543883985, -18.78004118034163739, 5.517608176248461227 ) ) ;
#4367 = ORIENTED_EDGE ( 'NONE', *, *, #2316, .T. ) ;
#4368 = DIRECTION ( 'NONE',  ( 1.000000000000000000, -0.000000000000000000, -0.000000000000000000 ) ) ;
#4369 = ORIENTED_EDGE ( 'NONE', *, *, #13574, .T. ) ;
#4370 = CARTESIAN_POINT ( 'NONE',  ( 2.645259258103298983, -10.28229522185712241, 2.672449792925449596 ) ) ;
#4371 = VECTOR ( 'NONE', #684, 1000.000000000000000 ) ;
#4372 = VECTOR ( 'NONE', #18464, 1000.000000000000000 ) ;
#4373 = ORIENTED_EDGE ( 'NONE', *, *, #4048, .F. ) ;
#4374 = DIRECTION ( 'NONE',  ( 0.000000000000000000, 1.000000000000000000, -0.000000000000000000 ) ) ;
#4375 = DIRECTION ( 'NONE',  ( 0.8660254037844415942, 0.4999999999999950040, -0.000000000000000000 ) ) ;
#4376 = EDGE_CURVE ( 'NONE', #9554, #3751, #13120, .T. ) ;
#4377 = CARTESIAN_POINT ( 'NONE',  ( -0.5631383031621635116, -9.864917468222230923, 1.622643865078341907 ) ) ;
#4378 = FACE_OUTER_BOUND ( 'NONE', #11821, .T. ) ;
#4379 = CARTESIAN_POINT ( 'NONE',  ( -25.29469207716615031, 0.000000000000000000, 1.000000000000000000 ) ) ;
#4380 = CARTESIAN_POINT ( 'NONE',  ( 7.619520639128047002, 9.000000000000001776, 1.000000000000000000 ) ) ;
#4381 = CARTESIAN_POINT ( 'NONE',  ( -9.999999999999996447, -34.99999999999999289, 1.000000000000000000 ) ) ;
#4382 = EDGE_CURVE ( 'NONE', #14130, #14133, #19518, .T. ) ;
#4383 = ADVANCED_FACE ( 'NONE', ( #5169 ), #14792, .T. ) ;
#4384 = CARTESIAN_POINT ( 'NONE',  ( 4.847191417683177406, -20.91377862118959285, 1.020995438708345082 ) ) ;
#4385 = CARTESIAN_POINT ( 'NONE',  ( -13.12529397353891270, 5.014845663890295846, 3.333333333333220239 ) ) ;
#4386 = CARTESIAN_POINT ( 'NONE',  ( -7.753441417683176518, -21.94931252712233061, 1.749999999999998446 ) ) ;
#4387 = VECTOR ( 'NONE', #11954, 1000.000000000000000 ) ;
#4388 = VECTOR ( 'NONE', #9336, 1000.000000000000000 ) ;
#4389 = ORIENTED_EDGE ( 'NONE', *, *, #5170, .F. ) ;
#4390 = CARTESIAN_POINT ( 'NONE',  ( 7.277808582316794173, -20.27099543870833642, 2.724438792969431589 ) ) ;
#4391 = CARTESIAN_POINT ( 'NONE',  ( -7.500000000000000000, -25.49999999999999645, 6.500000000000000000 ) ) ;
#4392 = CARTESIAN_POINT ( 'NONE',  ( -13.37607268932110038, -20.94582918928111681, 4.945564004704174010 ) ) ;
#4393 = CARTESIAN_POINT ( 'NONE',  ( 10.55905858231679595, -20.72672167713054137, 4.701595411283463477 ) ) ;
#4394 = PLANE ( 'NONE',  #2310 ) ;
#4395 = EDGE_LOOP ( 'NONE', ( #863, #72, #15191, #3914 ) ) ;
#4396 = ORIENTED_EDGE ( 'NONE', *, *, #15117, .F. ) ;
#4397 = CARTESIAN_POINT ( 'NONE',  ( 13.40322194933353828, -19.57479155865495457, 6.214283636730510096 ) ) ;
#4398 = LINE ( 'NONE', #6073, #6584 ) ;
#4399 = ORIENTED_EDGE ( 'NONE', *, *, #19975, .T. ) ;
#4400 = DIRECTION ( 'NONE',  ( 0.000000000000000000, -1.000000000000000000, 0.000000000000000000 ) ) ;
#4401 = ORIENTED_EDGE ( 'NONE', *, *, #17788, .T. ) ;
#4402 = CARTESIAN_POINT ( 'NONE',  ( -10.09030858231679595, -21.32581373872472597, 1.729004561291657582 ) ) ;
#4403 = AXIS2_PLACEMENT_3D ( 'NONE', #14938, #9165, #1323 ) ;
#4404 = CARTESIAN_POINT ( 'NONE',  ( 23.10856191738414012, 0.000000000000000000, 1.000000000000000000 ) ) ;
#4405 = EDGE_CURVE ( 'NONE', #8442, #20408, #8424, .T. ) ;
#4406 = DIRECTION ( 'NONE',  ( 0.000000000000000000, 0.000000000000000000, 1.000000000000000000 ) ) ;
#4407 = CARTESIAN_POINT ( 'NONE',  ( 1.819865260185086875, -9.122006307963404836, 1.624464420737683046 ) ) ;
#4408 = DIRECTION ( 'NONE',  ( 1.000000000000000000, 0.000000000000000000, 0.000000000000000000 ) ) ;
#4409 = CARTESIAN_POINT ( 'NONE',  ( -13.37930517931174634, -19.28258844475809042, 4.742233558278135419 ) ) ;
#4410 = CARTESIAN_POINT ( 'NONE',  ( 14.99999999999999645, 3.000000000000003553, 1.000000000000000000 ) ) ;
#4411 = CARTESIAN_POINT ( 'NONE',  ( -13.42074492158312715, -18.68988146005270679, 6.255046935864005064 ) ) ;
#4412 = CYLINDRICAL_SURFACE ( 'NONE', #19068, 0.3750000000000003331 ) ;
#4413 = CARTESIAN_POINT ( 'NONE',  ( 11.49655858231679417, -22.05068747287764452, 1.749999999999998446 ) ) ;
#4414 = EDGE_CURVE ( 'NONE', #9600, #17347, #10188, .T. ) ;
#4415 = AXIS2_PLACEMENT_3D ( 'NONE', #6463, #1537, #11362 ) ;
#4416 = CARTESIAN_POINT ( 'NONE',  ( 11.87844141768317741, -22.99999999999999645, 3.449312527122335048 ) ) ;
#4417 = CARTESIAN_POINT ( 'NONE',  ( -12.53469141768317741, -20.22900456129164581, 2.825813738724748170 ) ) ;
#4418 = VERTEX_POINT ( 'NONE', #15098 ) ;
#4419 = CARTESIAN_POINT ( 'NONE',  ( 13.09494140422671471, 4.232040913449062636, 5.131376921800749003 ) ) ;
#4420 = DIRECTION ( 'NONE',  ( 0.000000000000000000, 0.2487476929738665354, 0.9685683172808094987 ) ) ;
#4421 = ORIENTED_EDGE ( 'NONE', *, *, #14210, .F. ) ;
#4422 = ORIENTED_EDGE ( 'NONE', *, *, #17515, .F. ) ;
#4423 = DIRECTION ( 'NONE',  ( 1.000000000000000000, 0.000000000000000000, 0.000000000000000000 ) ) ;
#4424 = AXIS2_PLACEMENT_3D ( 'NONE', #18262, #15423, #8746 ) ;
#4425 = CARTESIAN_POINT ( 'NONE',  ( -12.62562019941893432, -20.21867992933967173, 4.757612834768309540 ) ) ;
#4426 = ADVANCED_FACE ( 'NONE', ( #10400 ), #4120, .T. ) ;
#4427 = ADVANCED_FACE ( 'NONE', ( #2860 ), #13622, .T. ) ;
#4428 = CARTESIAN_POINT ( 'NONE',  ( -1.904508877737772998, -9.138371295333994837, 2.378667276417936627 ) ) ;
#4429 = CARTESIAN_POINT ( 'NONE',  ( -13.87470602645761986, 4.985154336109792972, 4.666666666666619889 ) ) ;
#4430 = VECTOR ( 'NONE', #359, 1000.000000000000000 ) ;
#4431 = LINE ( 'NONE', #18454, #15397 ) ;
#4432 = CARTESIAN_POINT ( 'NONE',  ( -12.62500000000001954, -20.24999999999450040, 3.833333333368183382 ) ) ;
#4433 = DIRECTION ( 'NONE',  ( -0.000000000000000000, -0.000000000000000000, -1.000000000000000000 ) ) ;
#4434 = CARTESIAN_POINT ( 'NONE',  ( -11.24178095869206828, 4.999999999999999112, 1.000000000000000000 ) ) ;
#4435 = FACE_OUTER_BOUND ( 'NONE', #10331, .T. ) ;
#4436 = CARTESIAN_POINT ( 'NONE',  ( -10.93405858231679595, -23.73192549717337130, 5.303608408759367343 ) ) ;
#4437 = CARTESIAN_POINT ( 'NONE',  ( -2.801385037117921861, -10.23463596792102415, 1.910209944425432349 ) ) ;
#4438 = VERTEX_POINT ( 'NONE', #2540 ) ;
#4439 = CARTESIAN_POINT ( 'NONE',  ( -13.38450946332969771, -19.76977210184853462, 5.359796180098093998 ) ) ;
#4440 = VECTOR ( 'NONE', #19791, 1000.000000000000000 ) ;
#4441 = CARTESIAN_POINT ( 'NONE',  ( 12.00000000000000178, -18.50000000000000355, 4.000000000000000000 ) ) ;
#4442 = EDGE_CURVE ( 'NONE', #868, #5651, #4014, .T. ) ;
#4443 = CARTESIAN_POINT ( 'NONE',  ( 5.777808582316795949, -19.52099543870833642, 2.413778621189609286 ) ) ;
#4444 = CARTESIAN_POINT ( 'NONE',  ( -13.18405858231679595, -21.32873467460644079, 2.757051763020455404 ) ) ;
#4445 = ORIENTED_EDGE ( 'NONE', *, *, #4514, .F. ) ;
#4446 = CARTESIAN_POINT ( 'NONE',  ( 13.39782821820594627, -19.84717498059871943, 6.143582220458365661 ) ) ;
#4447 = CARTESIAN_POINT ( 'NONE',  ( 0.000000000000000000, 4.999999999999999112, 1.000000000000000000 ) ) ;
#4448 = ORIENTED_EDGE ( 'NONE', *, *, #2388, .T. ) ;
#4449 = VERTEX_POINT ( 'NONE', #12167 ) ;
#4450 = VECTOR ( 'NONE', #13495, 1000.000000000000000 ) ;
#4451 = CARTESIAN_POINT ( 'NONE',  ( -13.49999999999998401, -18.49999999999999645, 4.000000000000000000 ) ) ;
#4452 = ORIENTED_EDGE ( 'NONE', *, *, #18497, .F. ) ;
#4453 = CARTESIAN_POINT ( 'NONE',  ( -13.40382044110196347, -18.79456772435387890, 5.502763032956559108 ) ) ;
#4454 = CARTESIAN_POINT ( 'NONE',  ( 2.534747216115884161, -9.671180236796224960, 2.515503256513427210 ) ) ;
#4455 = EDGE_LOOP ( 'NONE', ( #19066, #3829, #8075, #8869 ) ) ;
#4456 = DIRECTION ( 'NONE',  ( 1.000000000000000000, -0.000000000000000000, -0.000000000000000000 ) ) ;
#4457 = CARTESIAN_POINT ( 'NONE',  ( -3.499999999999998668, -19.50000000000000000, 1.000000000000000000 ) ) ;
#4458 = FACE_OUTER_BOUND ( 'NONE', #8775, .T. ) ;
#4459 = CARTESIAN_POINT ( 'NONE',  ( 2.887553741010006281, -10.84643174835951207, 2.067331322690557638 ) ) ;
#4460 = CARTESIAN_POINT ( 'NONE',  ( -19.48630159782011262, 4.999999999999999112, 1.000000000000000000 ) ) ;
#4461 = CARTESIAN_POINT ( 'NONE',  ( 13.12529418130016445, 5.014856155665242454, 4.958178834604180629 ) ) ;
#4462 = AXIS2_PLACEMENT_3D ( 'NONE', #9255, #8666, #15626 ) ;
#4463 = CARTESIAN_POINT ( 'NONE',  ( 0.000000000000000000, 9.000000000000001776, 1.000000000000000000 ) ) ;
#4464 = CARTESIAN_POINT ( 'NONE',  ( 0.000000000000000000, 10.00000000000000000, 1.000000000000000000 ) ) ;
#4465 = DIRECTION ( 'NONE',  ( -1.000000000000000000, 0.000000000000000000, 0.000000000000000000 ) ) ;
#4466 = CARTESIAN_POINT ( 'NONE',  ( 5.690941417683177406, -22.74294823697955081, 4.171265325393542334 ) ) ;
#4467 = CARTESIAN_POINT ( 'NONE',  ( -13.10756170493883310, 4.119366099410778581, 6.001761809183453700 ) ) ;
#4468 = CARTESIAN_POINT ( 'NONE',  ( -8.965308582316795949, -20.97900456129165647, 3.863526089495444626 ) ) ;
#4469 = EDGE_CURVE ( 'NONE', #5740, #7202, #9236, .T. ) ;
#4470 = CARTESIAN_POINT ( 'NONE',  ( -4.284691417683177406, -24.52099543870834708, 4.484846433055073689 ) ) ;
#4471 = EDGE_LOOP ( 'NONE', ( #9775, #13409, #18137, #6655 ) ) ;
#4472 = CARTESIAN_POINT ( 'NONE',  ( 13.09560264576187905, 4.265433610975056133, 4.791666666666684726 ) ) ;
#4473 = DIRECTION ( 'NONE',  ( 1.000000000000000000, 0.000000000000000000, 0.000000000000000000 ) ) ;
#4474 = ORIENTED_EDGE ( 'NONE', *, *, #1110, .F. ) ;
#4475 = DIRECTION ( 'NONE',  ( 1.000000000000000000, 0.000000000000000000, 0.000000000000000000 ) ) ;
#4476 = VECTOR ( 'NONE', #1895, 1000.000000000000000 ) ;
#4477 = ORIENTED_EDGE ( 'NONE', *, *, #9972, .T. ) ;
#4478 = CARTESIAN_POINT ( 'NONE',  ( 2.513306525444908512, -9.622685169956881168, 2.503048754562789746 ) ) ;
#4479 = ORIENTED_EDGE ( 'NONE', *, *, #11903, .T. ) ;
#4480 = PLANE ( 'NONE',  #10654 ) ;
#4481 = CARTESIAN_POINT ( 'NONE',  ( -11.75209451496117197, 10.00000000000000000, 1.000000000000000000 ) ) ;
#4482 = CARTESIAN_POINT ( 'NONE',  ( -1.548630333695928618, -9.864917468222230923, 1.622643865078341907 ) ) ;
#4483 = CARTESIAN_POINT ( 'NONE',  ( -10.38119784648305632, -14.00000000000000000, 2.000000000000000000 ) ) ;
#4484 = DIRECTION ( 'NONE',  ( 0.000000000000000000, 0.000000000000000000, -1.000000000000000000 ) ) ;
#4485 = DIRECTION ( 'NONE',  ( 0.000000000000000000, 1.000000000000000000, -0.000000000000000000 ) ) ;
#4486 = CARTESIAN_POINT ( 'NONE',  ( 5.972191417683178294, -24.47900456129165292, 2.413778621189595963 ) ) ;
#4487 = CARTESIAN_POINT ( 'NONE',  ( -11.69094141768317563, -23.27327832286946219, 4.701595411283453707 ) ) ;
#4488 = ORIENTED_EDGE ( 'NONE', *, *, #15399, .F. ) ;
#4489 = CARTESIAN_POINT ( 'NONE',  ( 4.840308582316793284, -22.67418626127525982, 5.270995438708342640 ) ) ;
#4490 = CARTESIAN_POINT ( 'NONE',  ( 26.69203811574919882, 16.00000000000000000, 1.000000000000000000 ) ) ;
#4491 = CARTESIAN_POINT ( 'NONE',  ( -12.66503773474750894, -18.97809439524806052, 6.263381662489337920 ) ) ;
#4492 = VERTEX_POINT ( 'NONE', #17183 ) ;
#4493 = EDGE_CURVE ( 'NONE', #15313, #9004, #8407, .T. ) ;
#4494 = CARTESIAN_POINT ( 'NONE',  ( 7.746558582316794173, -21.94931252712234482, 5.250000000000000888 ) ) ;
#4495 = LINE ( 'NONE', #15472, #20697 ) ;
#4496 = VERTEX_POINT ( 'NONE', #18768 ) ;
#4497 = CARTESIAN_POINT ( 'NONE',  ( 13.85716935893578317, 3.349552626256921517, 6.729005269197402939 ) ) ;
#4498 = LINE ( 'NONE', #17151, #8234 ) ;
#4499 = SHAPE_REPRESENTATION_RELATIONSHIP ( 'NONE' , 'NONE' ,  #6161, #10808 ) ;
#4500 = ORIENTED_EDGE ( 'NONE', *, *, #1195, .F. ) ;
#4501 = CARTESIAN_POINT ( 'NONE',  ( -20.00349085826861995, 10.00000000000000000, 0.000000000000000000 ) ) ;
#4502 = ADVANCED_FACE ( 'NONE', ( #1092 ), #13731, .T. ) ;
#4503 = ORIENTED_EDGE ( 'NONE', *, *, #9517, .T. ) ;
#4504 = CARTESIAN_POINT ( 'NONE',  ( -12.05905858231679417, -20.72672167713054137, 4.701595411283463477 ) ) ;
#4505 = FACE_OUTER_BOUND ( 'NONE', #19271, .T. ) ;
#4506 = CARTESIAN_POINT ( 'NONE',  ( 25.04469207716615031, 4.999999999999999112, 0.000000000000000000 ) ) ;
#4507 = CARTESIAN_POINT ( 'NONE',  ( 3.049989092406311109, -8.938202327316346896, 1.769874869409437279 ) ) ;
#4508 = LINE ( 'NONE', #14016, #6343 ) ;
#4509 = CARTESIAN_POINT ( 'NONE',  ( -13.09560264575884503, 4.265433610975056133, 3.333333333333364568 ) ) ;
#4510 = CARTESIAN_POINT ( 'NONE',  ( 5.777808582316794173, -20.27099543870833642, 2.724438792969431589 ) ) ;
#4511 = CARTESIAN_POINT ( 'NONE',  ( -13.90439735423812273, 5.734566389025032684, 4.166666666666765551 ) ) ;
#4512 = CARTESIAN_POINT ( 'NONE',  ( -13.87500000000000000, 5.000000000000049738, 4.000000000000000888 ) ) ;
#4513 = CARTESIAN_POINT ( 'NONE',  ( 9.621558582316794173, -23.74999999999999645, 3.550687472877651629 ) ) ;
#4514 = EDGE_CURVE ( 'NONE', #7075, #5681, #15200, .T. ) ;
#4515 = CARTESIAN_POINT ( 'NONE',  ( 13.09030858231679417, -21.63647391050454871, 2.479004561291657804 ) ) ;
#4516 = CARTESIAN_POINT ( 'NONE',  ( -7.559058582316794173, -20.72672167713054137, 4.701595411283463477 ) ) ;
#4517 = VERTEX_POINT ( 'NONE', #13831 ) ;
#4518 = CARTESIAN_POINT ( 'NONE',  ( 13.37818000216760694, -19.33940989053615311, 4.728953261990445966 ) ) ;
#4519 = CARTESIAN_POINT ( 'NONE',  ( -2.777355782919915139, -10.06396397089670458, 1.866377966073868411 ) ) ;
#4520 = ORIENTED_EDGE ( 'NONE', *, *, #10684, .F. ) ;
#4521 = VERTEX_POINT ( 'NONE', #2441 ) ;
#4522 = DIRECTION ( 'NONE',  ( 3.469446951953619119E-16, 1.000000000000000000, -0.000000000000000000 ) ) ;
#4523 = CARTESIAN_POINT ( 'NONE',  ( -12.62499999999998224, -20.25000000000006395, 4.416666666666681174 ) ) ;
#4524 = VECTOR ( 'NONE', #5997, 1000.000000000000000 ) ;
#4525 = CARTESIAN_POINT ( 'NONE',  ( -0.9854920305337622199, -8.364917468222230923, 2.372643865078341019 ) ) ;
#4526 = CARTESIAN_POINT ( 'NONE',  ( -13.87470602645761986, 4.985154336109792972, 4.833333333333344584 ) ) ;
#4527 = ADVANCED_FACE ( 'NONE', ( #10817 ), #15299, .T. ) ;
#4528 = LINE ( 'NONE', #16137, #4388 ) ;
#4529 = CARTESIAN_POINT ( 'NONE',  ( -16.62779268661489951, 11.64110105645932691, 0.000000000000000000 ) ) ;
#4530 = CARTESIAN_POINT ( 'NONE',  ( 11.49655858231679417, -22.05068747287764452, 1.749999999999998446 ) ) ;
#4531 = CARTESIAN_POINT ( 'NONE',  ( -5.381197846483055436, -6.000000000000000000, 2.000000000000000000 ) ) ;
#4532 = CARTESIAN_POINT ( 'NONE',  ( 13.14123030749026277, 5.069630528265579805, 6.418963484850015000 ) ) ;
#4533 = CARTESIAN_POINT ( 'NONE',  ( -12.62155858231679417, -24.50000000000000000, 3.550687472877651629 ) ) ;
#4534 = CARTESIAN_POINT ( 'NONE',  ( -1.548630333695928618, -9.864917468222230923, 1.622643865078341907 ) ) ;
#4535 = ORIENTED_EDGE ( 'NONE', *, *, #2638, .F. ) ;
#4536 = CARTESIAN_POINT ( 'NONE',  ( -13.83710853266996388, 3.836480899831821834, 5.239411421715695738 ) ) ;
#4537 = DIRECTION ( 'NONE',  ( -0.000000000000000000, 0.000000000000000000, -1.000000000000000000 ) ) ;
#4538 = CARTESIAN_POINT ( 'NONE',  ( 11.50344141768317741, -22.05068747287766229, 6.000000000000001776 ) ) ;
#4539 = CARTESIAN_POINT ( 'NONE',  ( -11.59030858231679595, -21.63647391050454871, 2.479004561291657804 ) ) ;
#4540 = ORIENTED_EDGE ( 'NONE', *, *, #448, .F. ) ;
#4541 = EDGE_CURVE ( 'NONE', #13777, #1443, #1292, .T. ) ;
#4542 = CARTESIAN_POINT ( 'NONE',  ( 13.87454419214980739, 4.976981703567351367, 5.131312659523921127 ) ) ;
#4543 = DIRECTION ( 'NONE',  ( 0.000000000000000000, 1.000000000000000000, 0.000000000000000000 ) ) ;
#4544 = VERTEX_POINT ( 'NONE', #1191 ) ;
#4545 = VECTOR ( 'NONE', #17648, 1000.000000000000000 ) ;
#4546 = ORIENTED_EDGE ( 'NONE', *, *, #19785, .F. ) ;
#4547 = DIRECTION ( 'NONE',  ( 0.000000000000000000, 1.000000000000000000, -0.000000000000000000 ) ) ;
#4548 = ORIENTED_EDGE ( 'NONE', *, *, #174, .F. ) ;
#4549 = CARTESIAN_POINT ( 'NONE',  ( -13.41820805991576826, -18.06799297425606454, 5.518388032956592859 ) ) ;
#4550 = LINE ( 'NONE', #9358, #12797 ) ;
#4551 = CARTESIAN_POINT ( 'NONE',  ( 14.31494360078803041, 0.000000000000000000, 1.000000000000000000 ) ) ;
#4552 = CARTESIAN_POINT ( 'NONE',  ( -27.00000000000000000, 0.000000000000000000, 0.000000000000000000 ) ) ;
#4553 = CARTESIAN_POINT ( 'NONE',  ( 2.559937518207947793, -9.746075135043517079, 2.534737762559237773 ) ) ;
#4554 = DIRECTION ( 'NONE',  ( 1.000000000000000000, 2.312964634635731617E-15, 0.000000000000000000 ) ) ;
#4555 = CARTESIAN_POINT ( 'NONE',  ( 1.619022621591186928, -8.364917468222230923, 1.622643865078341907 ) ) ;
#4556 = DIRECTION ( 'NONE',  ( 0.000000000000000000, 0.000000000000000000, 1.000000000000000000 ) ) ;
#4557 = CARTESIAN_POINT ( 'NONE',  ( 13.12529397354238192, 5.014845663890295846, 4.333333333333382775 ) ) ;
#4558 = DIRECTION ( 'NONE',  ( -1.000000000000000000, 0.000000000000000000, 0.000000000000000000 ) ) ;
#4559 = PLANE ( 'NONE',  #4694 ) ;
#4560 = CARTESIAN_POINT ( 'NONE',  ( 17.30017143803810242, 0.000000000000000000, 1.000000000000000000 ) ) ;
#4561 = CARTESIAN_POINT ( 'NONE',  ( 7.472191417683177406, -22.97900456129165292, 3.035098964749240125 ) ) ;
#4562 = CARTESIAN_POINT ( 'NONE',  ( -12.79798428357658047, -11.51429367935891790, 5.673858176248284479 ) ) ;
#4563 = CARTESIAN_POINT ( 'NONE',  ( -8.590308582316797725, -21.63647391050454871, 2.479004561291657804 ) ) ;
#4564 = CARTESIAN_POINT ( 'NONE',  ( -11.03469141768318273, -20.22900456129164581, 2.825813738724747726 ) ) ;
#4565 = EDGE_LOOP ( 'NONE', ( #2551, #17946, #2660, #8051, #10413, #15479, #2556, #15901, #16681, #14107, #18364, #4132, #8765, #19552, #20439, #8772, #707, #14031, #14827, #15809, #19870, #12680, #582, #14440, #6785, #4610, #9110, #15762, #15213, #3157, #11006, #12841, #10328, #17635, #15904, #7765, #9075, #8130, #940, #9839, #16813, #12721, #5053, #8416, #984, #2507, #18132, #19871, #12586, #6552, #1815, #6968, #7689, #4287, #820, #5910, #2398, #3358, #14949, #6127, #1670, #17920, #5839, #15957, #8603, #5384, #7574, #3409, #7579, #2852, #19350, #19861, #17351, #91, #20149, #9329, #8176, #5211, #1751, #12786, #6009, #3534, #1540, #11108, #5493, #5091, #18646, #14009, #9406, #13160, #11166, #16785, #13231, #7485, #8528, #6682, #126, #13904, #11379, #16962, #20636, #12556, #16675, #11375, #3257, #3925, #14301, #16477, #7864, #121, #10126, #10129, #8938, #3899, #8318, #6215, #18209, #15122, #4548, #5235, #17611, #305, #13384, #18492 ) ) ;
#4566 = ADVANCED_FACE ( 'NONE', ( #18457 ), #18658, .T. ) ;
#4567 = CARTESIAN_POINT ( 'NONE',  ( 13.09080647246885576, 4.023226859705822278, 5.257958009367514229 ) ) ;
#4568 = DIRECTION ( 'NONE',  ( 0.000000000000000000, 0.000000000000000000, 1.000000000000000000 ) ) ;
#4569 = ORIENTED_EDGE ( 'NONE', *, *, #3849, .F. ) ;
#4570 = DIRECTION ( 'NONE',  ( 0.000000000000000000, 1.000000000000000000, 0.000000000000000000 ) ) ;
#4571 = ORIENTED_EDGE ( 'NONE', *, *, #8544, .F. ) ;
#4572 = CARTESIAN_POINT ( 'NONE',  ( 1.732184490400474175, -9.869581059509965115, 2.373841568485653308 ) ) ;
#4573 = EDGE_LOOP ( 'NONE', ( #7624, #4138, #18621, #13413 ) ) ;
#4574 = CARTESIAN_POINT ( 'NONE',  ( 11.87844141768317563, -23.74999999999999645, 3.449312527122335492 ) ) ;
#4575 = EDGE_CURVE ( 'NONE', #16197, #10885, #7671, .T. ) ;
#4576 = CARTESIAN_POINT ( 'NONE',  ( -0.000000000000000000, 10.00000000000000000, 0.000000000000000000 ) ) ;
#4577 = CARTESIAN_POINT ( 'NONE',  ( 0.000000000000000000, -9.114917468222230923, 1.622643865078341019 ) ) ;
#4578 = DIRECTION ( 'NONE',  ( -0.000000000000000000, 0.000000000000000000, -1.000000000000000000 ) ) ;
#4579 = LINE ( 'NONE', #7521, #5635 ) ;
#4580 = VECTOR ( 'NONE', #12544, 1000.000000000000000 ) ;
#4581 = CARTESIAN_POINT ( 'NONE',  ( 5.034691417683177406, -19.47900456129164581, 2.515153566944927199 ) ) ;
#4582 = CARTESIAN_POINT ( 'NONE',  ( 15.06494360078803041, 0.000000000000000000, 1.000000000000000000 ) ) ;
#4583 = CARTESIAN_POINT ( 'NONE',  ( -12.62844141768317741, -20.24999999999999289, 3.550687472877664952 ) ) ;
#4584 = ORIENTED_EDGE ( 'NONE', *, *, #16503, .T. ) ;
#4585 = CARTESIAN_POINT ( 'NONE',  ( 8.309058582316792396, -23.27327832286945153, 2.298404588716537411 ) ) ;
#4586 = CARTESIAN_POINT ( 'NONE',  ( 7.500000000000000000, -24.49999999999999289, 4.000000000000000000 ) ) ;
#4587 = CARTESIAN_POINT ( 'NONE',  ( -12.70700162295422864, -16.85891804079483691, 6.308954579156044851 ) ) ;
#4588 = CARTESIAN_POINT ( 'NONE',  ( 11.99178095869207006, 4.999999999999999112, 0.000000000000000000 ) ) ;
#4589 = CARTESIAN_POINT ( 'NONE',  ( 14.50000000000001243, -25.49999999999999645, 1.000000000000000000 ) ) ;
#4590 = EDGE_LOOP ( 'NONE', ( #7386, #18778, #10107, #12587 ) ) ;
#4591 = CARTESIAN_POINT ( 'NONE',  ( -0.1250000000000001110, 16.00000000000000000, 1.000000000000000000 ) ) ;
#4592 = VERTEX_POINT ( 'NONE', #979 ) ;
#4593 = DIRECTION ( 'NONE',  ( 0.000000000000000000, 0.000000000000000000, 1.000000000000000000 ) ) ;
#4594 = VERTEX_POINT ( 'NONE', #10599 ) ;
#4595 = CARTESIAN_POINT ( 'NONE',  ( -9.246558582316794173, -21.94931252712234482, 5.250000000000000888 ) ) ;
#4596 = CARTESIAN_POINT ( 'NONE',  ( 12.62515553039088090, -20.24214571525854467, 4.629702272822510345 ) ) ;
#4597 = DIRECTION ( 'NONE',  ( -0.000000000000000000, -0.000000000000000000, -1.000000000000000000 ) ) ;
#4598 = CARTESIAN_POINT ( 'NONE',  ( 2.067263844777544435, -10.27417889452513933, 1.727750375171331676 ) ) ;
#4599 = AXIS2_PLACEMENT_3D ( 'NONE', #6598, #19668, #19782 ) ;
#4600 = ADVANCED_FACE ( 'NONE', ( #13932 ), #16973, .F. ) ;
#4601 = DIRECTION ( 'NONE',  ( 0.000000000000000000, 1.000000000000000000, 0.000000000000000000 ) ) ;
#4602 = CARTESIAN_POINT ( 'NONE',  ( -13.38007464613909470, -19.24373036997283037, 4.743072998953621777 ) ) ;
#4603 = CARTESIAN_POINT ( 'NONE',  ( 8.121558582316792396, -23.74999999999999645, 3.550687472877651629 ) ) ;
#4604 = CARTESIAN_POINT ( 'NONE',  ( -12.64183575740756993, -20.14979425091403087, 6.022201559249563907 ) ) ;
#4605 = DIRECTION ( 'NONE',  ( 1.000000000000000000, 0.000000000000000000, 0.000000000000000000 ) ) ;
#4606 = CARTESIAN_POINT ( 'NONE',  ( 9.434058582316794173, -23.20159541128345992, 4.773278322869455970 ) ) ;
#4607 = CARTESIAN_POINT ( 'NONE',  ( 6.065941417683177406, -22.67126532539353789, 2.757051763020445634 ) ) ;
#4608 = CARTESIAN_POINT ( 'NONE',  ( -10.75344141768317741, -21.94931252712233061, 1.749999999999998446 ) ) ;
#4609 = MECHANICAL_DESIGN_GEOMETRIC_PRESENTATION_REPRESENTATION (  '', ( #8290 ), #10966 ) ;
#4610 = ORIENTED_EDGE ( 'NONE', *, *, #14523, .F. ) ;
#4611 = CARTESIAN_POINT ( 'NONE',  ( 13.09560264576187905, 4.265433610975056133, 2.999999999999999556 ) ) ;
#4612 = CARTESIAN_POINT ( 'NONE',  ( -2.768424032093183662, -10.00067216410020166, 1.850123365707658785 ) ) ;
#4613 = ORIENTED_EDGE ( 'NONE', *, *, #11067, .T. ) ;
#4614 = PRODUCT_DEFINITION_CONTEXT ( 'detailed design', #1200, 'design' ) ;
#4615 = ORIENTED_EDGE ( 'NONE', *, *, #13480, .T. ) ;
#4616 = CARTESIAN_POINT ( 'NONE',  ( 7.499999999999999112, -18.49999999999999645, 6.500000000000000888 ) ) ;
#4617 = FACE_OUTER_BOUND ( 'NONE', #13878, .T. ) ;
#4618 = CLOSED_SHELL ( 'NONE', ( #14787, #4600, #3975, #6083, #20544, #1566, #12111, #12984, #16950, #8664, #4427, #15438, #4621, #13987, #1087, #20695, #14302, #4174, #17530, #13034, #20279, #15086, #6436, #1829, #16008, #4566, #10902, #36, #1103, #5264, #13456, #20399, #15396, #14857, #10042, #10284, #20268, #17488, #10143, #264, #8087, #14961, #9908, #8312, #16949, #20523, #10297, #3588, #5315, #12730, #4903, #9487, #4814, #20253, #2003, #16741, #15835, #12845, #6122, #9999, #12283, #1015, #12958, #13443, #3300, #7587, #14140, #920, #12803, #14253, #10904, #19991, #833, #9242, #3824, #5135, #3239, #2131, #17322, #3480, #12210, #11729, #6228, #18949, #19828, #16878, #3859, #11447, #6611, #12567, #16321, #10414, #18240, #461, #12671, #9031, #20120, #3151, #11174, #289, #19151, #5475, #14078, #9780, #11286, #9758, #20504, #18255, #7195, #8386, #897, #1197, #10043, #14094, #4896, #13030, #20616, #11313, #15289, #5935, #12284, #2309, #12427, #1240, #10941, #7909, #6464, #11463, #14587, #5743, #4787, #17462, #8597, #7569, #15408, #1471, #16110, #6550 ) ) ;
#4619 = CARTESIAN_POINT ( 'NONE',  ( -3.317048600639548095, -9.800042196285016161, 2.741212564741740465 ) ) ;
#4620 = CARTESIAN_POINT ( 'NONE',  ( -13.85403523778986390, 3.941279508358651817, 5.991705257707216958 ) ) ;
#4621 = ADVANCED_FACE ( 'NONE', ( #18351 ), #5894, .T. ) ;
#4622 = VECTOR ( 'NONE', #8903, 1000.000000000000000 ) ;
#4623 = CARTESIAN_POINT ( 'NONE',  ( 2.747777887823422471, -9.906471667804277459, 1.825930796414880763 ) ) ;
#4624 = CARTESIAN_POINT ( 'NONE',  ( 22.56633994409548194, 10.00000000000000000, 1.000000000000000000 ) ) ;
#4625 = CARTESIAN_POINT ( 'NONE',  ( 11.40280858231679595, -22.77556120703056308, 1.770995438708340197 ) ) ;
#4626 = FACE_OUTER_BOUND ( 'NONE', #8654, .T. ) ;
#4627 = CARTESIAN_POINT ( 'NONE',  ( 13.11862022235054503, 3.927821228673052723, 6.755987001683414483 ) ) ;
#4628 = CARTESIAN_POINT ( 'NONE',  ( -4.746558582316795061, -21.94931252712234127, 6.000000000000001776 ) ) ;
#4629 = CARTESIAN_POINT ( 'NONE',  ( -1.716273078461125090, -9.866787073280026021, 2.373124017006284170 ) ) ;
#4630 = EDGE_CURVE ( 'NONE', #9608, #10392, #12373, .T. ) ;
#4631 = VERTEX_POINT ( 'NONE', #14558 ) ;
#4632 = ADVANCED_FACE ( 'NONE', ( #17492 ), #7974, .F. ) ;
#4633 = CARTESIAN_POINT ( 'NONE',  ( -13.83411111208379474, 3.685111160228107252, 5.236156213382356484 ) ) ;
#4634 = CARTESIAN_POINT ( 'NONE',  ( -0.000000000000000000, 11.64110105645932691, 0.000000000000000000 ) ) ;
#4635 = CARTESIAN_POINT ( 'NONE',  ( 4.097191417683177406, -23.08622137881040359, 5.979004561291654696 ) ) ;
#4636 = CARTESIAN_POINT ( 'NONE',  ( -5.409691417683178294, -21.63647391050456648, 4.520995438708348857 ) ) ;
#4637 = EDGE_LOOP ( 'NONE', ( #14176, #5450, #16840, #20274 ) ) ;
#4638 = VECTOR ( 'NONE', #10343, 1000.000000000000000 ) ;
#4639 = CARTESIAN_POINT ( 'NONE',  ( 13.40432071140796744, -19.51930407389869515, 6.223619713037471968 ) ) ;
#4640 = LINE ( 'NONE', #6011, #17395 ) ;
#4641 = LINE ( 'NONE', #148, #16024 ) ;
#4642 = VERTEX_POINT ( 'NONE', #12571 ) ;
#4643 = ORIENTED_EDGE ( 'NONE', *, *, #13693, .F. ) ;
#4644 = LINE ( 'NONE', #20566, #18127 ) ;
#4645 = CARTESIAN_POINT ( 'NONE',  ( 0.000000000000000000, 10.00000000000000000, 1.000000000000000000 ) ) ;
#4646 = ORIENTED_EDGE ( 'NONE', *, *, #10516, .F. ) ;
#4647 = CARTESIAN_POINT ( 'NONE',  ( -15.49999999999998224, -17.49999999999999645, 4.000000000000000000 ) ) ;
#4648 = DIRECTION ( 'NONE',  ( -0.000000000000000000, -0.000000000000000000, -1.000000000000000000 ) ) ;
#4649 = EDGE_CURVE ( 'NONE', #14875, #17347, #8192, .T. ) ;
#4650 = VECTOR ( 'NONE', #19637, 1000.000000000000000 ) ;
#4651 = CARTESIAN_POINT ( 'NONE',  ( 13.87500000000000000, 4.995017896875348917, 3.999999999999998224 ) ) ;
#4652 = AXIS2_PLACEMENT_3D ( 'NONE', #6130, #1118, #13757 ) ;
#4653 = CARTESIAN_POINT ( 'NONE',  ( 2.780192134145684779, -10.08406280675441735, 1.871539748636713130 ) ) ;
#4654 = FACE_OUTER_BOUND ( 'NONE', #1403, .T. ) ;
#4655 = DIRECTION ( 'NONE',  ( 0.000000000000000000, 0.000000000000000000, -1.000000000000000000 ) ) ;
#4656 = AXIS2_PLACEMENT_3D ( 'NONE', #17016, #1721, #17503 ) ;
#4657 = CARTESIAN_POINT ( 'NONE',  ( -7.499999999999999112, -19.49999999999999645, 4.000000000000000000 ) ) ;
#4658 = CARTESIAN_POINT ( 'NONE',  ( -13.27780858231679595, -20.27099543870833642, 2.724438792969431589 ) ) ;
#4659 = CARTESIAN_POINT ( 'NONE',  ( -2.567175533087980188, -9.771398394011347577, 2.541241281345096859 ) ) ;
#4660 = VECTOR ( 'NONE', #10945, 1000.000000000000000 ) ;
#4661 = CARTESIAN_POINT ( 'NONE',  ( 4.847191417683177406, -21.53509896474923835, 2.520995438708346192 ) ) ;
#4662 = CARTESIAN_POINT ( 'NONE',  ( -12.62499999999998224, -19.49999999999998934, 4.166666666666637653 ) ) ;
#4663 = CARTESIAN_POINT ( 'NONE',  ( -12.15280858231679950, -21.53509896474924901, 4.479004561291659137 ) ) ;
#4664 = CARTESIAN_POINT ( 'NONE',  ( -6.159691417683175629, -22.98484643305507191, 0.9790045612916508100 ) ) ;
#4665 = ORIENTED_EDGE ( 'NONE', *, *, #9662, .T. ) ;
#4666 = CARTESIAN_POINT ( 'NONE',  ( 13.09001666039658573, 3.983341349998239966, 5.257104358157307367 ) ) ;
#4667 = PLANE ( 'NONE',  #6 ) ;
#4668 = VERTEX_POINT ( 'NONE', #19185 ) ;
#4669 = EDGE_CURVE ( 'NONE', #7911, #7740, #1807, .T. ) ;
#4670 = PLANE ( 'NONE',  #2964 ) ;
#4671 = ORIENTED_EDGE ( 'NONE', *, *, #14597, .F. ) ;
#4672 = CARTESIAN_POINT ( 'NONE',  ( 2.817596665886821672, -11.50588678273290988, 2.986692549455723267 ) ) ;
#4673 = VECTOR ( 'NONE', #12670, 1000.000000000000000 ) ;
#4674 = ORIENTED_EDGE ( 'NONE', *, *, #7490, .T. ) ;
#4675 = CARTESIAN_POINT ( 'NONE',  ( 9.534691417683177406, -20.22900456129164581, 2.825813738724748170 ) ) ;
#4676 = DIRECTION ( 'NONE',  ( 0.000000000000000000, 0.000000000000000000, 1.000000000000000000 ) ) ;
#4677 = EDGE_CURVE ( 'NONE', #11061, #12047, #14236, .T. ) ;
#4678 = EDGE_CURVE ( 'NONE', #14879, #19147, #137, .T. ) ;
#4679 = CARTESIAN_POINT ( 'NONE',  ( -2.594671182134835163, -9.923034775318452461, 2.580184533305832861 ) ) ;
#4680 = CARTESIAN_POINT ( 'NONE',  ( 23.10856191738414012, 0.000000000000000000, 0.000000000000000000 ) ) ;
#4681 = CARTESIAN_POINT ( 'NONE',  ( -9.902808582316794173, -22.77556120703056308, 1.770995438708340197 ) ) ;
#4682 = AXIS2_PLACEMENT_3D ( 'NONE', #8423, #19517, #16657 ) ;
#4683 = CARTESIAN_POINT ( 'NONE',  ( -20.49999999999998224, -21.99999999999999645, 9.999999999999998224 ) ) ;
#4684 = CARTESIAN_POINT ( 'NONE',  ( 4.097191417683177406, -23.08622137881040359, 5.979004561291654696 ) ) ;
#4685 = DIRECTION ( 'NONE',  ( -0.000000000000000000, -0.000000000000000000, -1.000000000000000000 ) ) ;
#4686 = CARTESIAN_POINT ( 'NONE',  ( -11.59719141768317563, -22.77556120703057729, 5.229004561291655584 ) ) ;
#4687 =( BOUNDED_CURVE ( )  B_SPLINE_CURVE ( 3, ( #1380, #15800, #1683, #17260 ),
 .UNSPECIFIED., .F., .T. ) 
 B_SPLINE_CURVE_WITH_KNOTS ( ( 4, 4 ),
 ( 0.5000000000000000000, 0.7500000000000000000 ),
 .UNSPECIFIED. ) 
 CURVE ( )  GEOMETRIC_REPRESENTATION_ITEM ( )  RATIONAL_B_SPLINE_CURVE ( ( 0.9667580569362952403, 0.6445053712908636045, 0.4833790284681485083, 0.4833790284681493410 ) ) 
 REPRESENTATION_ITEM ( '' )  );
#4688 = ORIENTED_EDGE ( 'NONE', *, *, #1, .T. ) ;
#4689 = CARTESIAN_POINT ( 'NONE',  ( 9.059058582316794173, -20.72672167713054137, 4.701595411283463477 ) ) ;
#4690 = DIRECTION ( 'NONE',  ( 0.000000000000000000, 0.000000000000000000, 1.000000000000000000 ) ) ;
#4691 = CARTESIAN_POINT ( 'NONE',  ( -12.62505438222622622, -20.99725369757571869, 4.613400783263607252 ) ) ;
#4692 = EDGE_LOOP ( 'NONE', ( #6173, #5109, #5987, #15010 ) ) ;
#4693 = ADVANCED_FACE ( 'NONE', ( #12783 ), #3269, .T. ) ;
#4694 = AXIS2_PLACEMENT_3D ( 'NONE', #12294, #10628, #7703 ) ;
#4695 = CARTESIAN_POINT ( 'NONE',  ( 13.42791111847407848, 0.000000000000000000, 1.000000000000000000 ) ) ;
#4696 = CARTESIAN_POINT ( 'NONE',  ( 10.00000000000000533, -30.00000000000000355, 1.000000000000000000 ) ) ;
#4697 = VERTEX_POINT ( 'NONE', #9645 ) ;
#4698 = DIRECTION ( 'NONE',  ( 0.000000000000000000, 0.000000000000000000, 1.000000000000000000 ) ) ;
#4699 = VERTEX_POINT ( 'NONE', #17278 ) ;
#4700 = DIRECTION ( 'NONE',  ( -0.000000000000000000, -0.000000000000000000, -1.000000000000000000 ) ) ;
#4701 = ORIENTED_EDGE ( 'NONE', *, *, #17294, .T. ) ;
#4702 = CARTESIAN_POINT ( 'NONE',  ( -11.21530858231679595, -24.52099543870834708, 2.515153566944913432 ) ) ;
#4703 = DIRECTION ( 'NONE',  ( 0.000000000000000000, -1.000000000000000000, 0.000000000000000000 ) ) ;
#4704 = VECTOR ( 'NONE', #1272, 1000.000000000000000 ) ;
#4705 = CARTESIAN_POINT ( 'NONE',  ( 11.00000000000000000, -25.49999999999999645, 4.000000000000000000 ) ) ;
#4706 = CARTESIAN_POINT ( 'NONE',  ( 1.337453470010121714, -9.114917468222230923, 1.622643865078341463 ) ) ;
#4707 = VECTOR ( 'NONE', #8845, 1000.000000000000000 ) ;
#4708 = VECTOR ( 'NONE', #3707, 1000.000000000000000 ) ;
#4709 = VECTOR ( 'NONE', #16028, 1000.000000000000000 ) ;
#4710 = LINE ( 'NONE', #19776, #11035 ) ;
#4711 = CARTESIAN_POINT ( 'NONE',  ( -13.83531008031826026, 3.745659056069631898, 5.237458296715707284 ) ) ;
#4712 = CARTESIAN_POINT ( 'NONE',  ( 13.27780858231679417, -19.52099543870833642, 2.413778621189609286 ) ) ;
#4713 = CARTESIAN_POINT ( 'NONE',  ( -12.62499999999998224, -20.99999999999998934, 4.166666666666637653 ) ) ;
#4714 = LINE ( 'NONE', #10998, #19436 ) ;
#4715 = FACE_OUTER_BOUND ( 'NONE', #2927, .T. ) ;
#4716 = EDGE_CURVE ( 'NONE', #1688, #12251, #15818, .T. ) ;
#4717 = CARTESIAN_POINT ( 'NONE',  ( 4.472191417683178294, -22.97900456129165292, 3.035098964749240125 ) ) ;
#4718 = CARTESIAN_POINT ( 'NONE',  ( -6.059058582316793284, -20.72672167713054137, 4.701595411283463477 ) ) ;
#4719 = ORIENTED_EDGE ( 'NONE', *, *, #5705, .F. ) ;
#4720 = CARTESIAN_POINT ( 'NONE',  ( 13.09560260347216953, 4.265431475339161338, 5.020858537328734883 ) ) ;
#4721 = VECTOR ( 'NONE', #1785, 1000.000000000000000 ) ;
#4722 = DIRECTION ( 'NONE',  ( -1.000000000000000000, 0.000000000000000000, 0.000000000000000000 ) ) ;
#4723 = ORIENTED_EDGE ( 'NONE', *, *, #15494, .F. ) ;
#4724 = VECTOR ( 'NONE', #6752, 999.9999999999998863 ) ;
#4725 = ORIENTED_EDGE ( 'NONE', *, *, #15911, .T. ) ;
#4726 = LINE ( 'NONE', #222, #1108 ) ;
#4727 = CARTESIAN_POINT ( 'NONE',  ( -13.12270769621861355, 4.884238659038159902, 5.513847264053151065 ) ) ;
#4728 = AXIS2_PLACEMENT_3D ( 'NONE', #365, #6751, #5267 ) ;
#4729 = CARTESIAN_POINT ( 'NONE',  ( -3.607313482701580476, -10.70492285834919244, 2.223603995567122293 ) ) ;
#4730 = DIRECTION ( 'NONE',  ( 0.000000000000000000, -0.000000000000000000, 1.000000000000000000 ) ) ;
#4731 = CARTESIAN_POINT ( 'NONE',  ( 2.589709240944451096, -9.559844081062008669, 1.736909907557668165 ) ) ;
#4732 = CARTESIAN_POINT ( 'NONE',  ( -12.64931222250080545, -19.02223276370786209, 5.512399842915133519 ) ) ;
#4733 = CARTESIAN_POINT ( 'NONE',  ( 12.80905858231679417, -23.27327832286945153, 2.298404588716537411 ) ) ;
#4734 = DIRECTION ( 'NONE',  ( 0.000000000000000000, 1.000000000000000000, 0.000000000000000000 ) ) ;
#4735 = CARTESIAN_POINT ( 'NONE',  ( 13.15316049959406364, 5.672105229501871904, 5.573635960501007958 ) ) ;
#4736 = AXIS2_PLACEMENT_3D ( 'NONE', #20708, #15776, #18828 ) ;
#4737 = AXIS2_PLACEMENT_3D ( 'NONE', #8635, #891, #15007 ) ;
#4738 = CARTESIAN_POINT ( 'NONE',  ( -2.110348196723525138, -10.58007678474401914, 1.806311064303893099 ) ) ;
#4739 = VERTEX_POINT ( 'NONE', #2962 ) ;
#4740 = CARTESIAN_POINT ( 'NONE',  ( -13.87470602645761986, 4.985154336109792972, 4.833333333333344584 ) ) ;
#4741 = DIRECTION ( 'NONE',  ( 0.000000000000000000, -1.000000000000000000, 0.000000000000000000 ) ) ;
#4742 = CARTESIAN_POINT ( 'NONE',  ( 12.25344141768317741, -21.94931252712233061, 1.749999999999998446 ) ) ;
#4743 = CARTESIAN_POINT ( 'NONE',  ( -5.034691417683177406, -20.97900456129164581, 3.136473910504570917 ) ) ;
#4744 = ORIENTED_EDGE ( 'NONE', *, *, #13240, .F. ) ;
#4745 = CARTESIAN_POINT ( 'NONE',  ( 13.37671366598624800, -20.91345986769124465, 5.053911344471881506 ) ) ;
#4746 = CARTESIAN_POINT ( 'NONE',  ( 0.000000000000000000, 9.000000000000001776, 0.000000000000000000 ) ) ;
#4747 = DIRECTION ( 'NONE',  ( 1.000000000000000000, 0.000000000000000000, 0.000000000000000000 ) ) ;
#4748 = EDGE_LOOP ( 'NONE', ( #3561, #12688, #9884, #8177, #19560 ) ) ;
#4749 = EDGE_CURVE ( 'NONE', #14732, #17662, #7058, .T. ) ;
#4750 = EDGE_LOOP ( 'NONE', ( #8302, #6285, #8715, #4399 ) ) ;
#4751 = CARTESIAN_POINT ( 'NONE',  ( -5.999999999999999112, -7.500000000000047073, 2.000000000000000000 ) ) ;
#4752 = VECTOR ( 'NONE', #15843, 1000.000000000000000 ) ;
#4753 = CARTESIAN_POINT ( 'NONE',  ( -14.49999999999998579, -24.49999999999999289, 4.000000000000000000 ) ) ;
#4754 = EDGE_CURVE ( 'NONE', #382, #14114, #4940, .T. ) ;
#4755 = EDGE_CURVE ( 'NONE', #18278, #3865, #18870, .T. ) ;
#4756 = DIRECTION ( 'NONE',  ( 1.000000000000000000, 0.000000000000000000, 0.000000000000000000 ) ) ;
#4757 = CARTESIAN_POINT ( 'NONE',  ( 2.579281110863027582, -9.822567596814183233, 2.554382554832406615 ) ) ;
#4758 = PLANE ( 'NONE',  #639 ) ;
#4759 = CARTESIAN_POINT ( 'NONE',  ( 2.762374231067749708, -9.968169115173667549, 1.841775933429679268 ) ) ;
#4760 = DIRECTION ( 'NONE',  ( -1.000000000000000000, 2.312964634635752916E-15, 0.000000000000000000 ) ) ;
#4761 = FACE_OUTER_BOUND ( 'NONE', #14309, .T. ) ;
#4762 = LINE ( 'NONE', #11147, #3352 ) ;
#4763 = LINE ( 'NONE', #3198, #7970 ) ;
#4764 = CARTESIAN_POINT ( 'NONE',  ( -12.99655858231679417, -22.05068747287764452, 1.749999999999998446 ) ) ;
#4765 = CARTESIAN_POINT ( 'NONE',  ( -1.513434189748285696, -9.114917468222230923, 2.372643865078341019 ) ) ;
#4766 = CARTESIAN_POINT ( 'NONE',  ( 13.37155858231679595, -20.99999999999999645, 3.449312527122348371 ) ) ;
#4767 = CARTESIAN_POINT ( 'NONE',  ( -13.12503131243110843, 5.001581277770153378, 5.166347330538456184 ) ) ;
#4768 = CARTESIAN_POINT ( 'NONE',  ( -11.87155858231679417, -20.24999999999999289, 3.449312527122348371 ) ) ;
#4769 = VECTOR ( 'NONE', #14335, 1000.000000000000000 ) ;
#4770 = CARTESIAN_POINT ( 'NONE',  ( -4.565941417683176518, -23.73192549717336064, 1.696391591240623331 ) ) ;
#4771 = ORIENTED_EDGE ( 'NONE', *, *, #11475, .F. ) ;
#4772 = CARTESIAN_POINT ( 'NONE',  ( 13.08799567112409790, 3.881281391764801025, 5.254907606674271037 ) ) ;
#4773 = LINE ( 'NONE', #19624, #2358 ) ;
#4774 = ORIENTED_EDGE ( 'NONE', *, *, #15250, .F. ) ;
#4775 = ORIENTED_EDGE ( 'NONE', *, *, #1308, .T. ) ;
#4776 = FACE_OUTER_BOUND ( 'NONE', #11745, .T. ) ;
#4777 = EDGE_CURVE ( 'NONE', #5036, #19990, #1594, .T. ) ;
#4778 = ORIENTED_EDGE ( 'NONE', *, *, #3127, .F. ) ;
#4779 = CARTESIAN_POINT ( 'NONE',  ( 19.19064177244175440, 10.00000000000000000, 0.000000000000000000 ) ) ;
#4780 = VERTEX_POINT ( 'NONE', #3376 ) ;
#4781 = DIRECTION ( 'NONE',  ( 0.000000000000000000, 0.2487476929738665354, 0.9685683172808094987 ) ) ;
#4782 = AXIS2_PLACEMENT_3D ( 'NONE', #6172, #4593, #19046 ) ;
#4783 = DIRECTION ( 'NONE',  ( 0.000000000000000000, -0.000000000000000000, 1.000000000000000000 ) ) ;
#4784 = CARTESIAN_POINT ( 'NONE',  ( -1.619022621591186928, -9.864917468222230923, 2.372643865078341019 ) ) ;
#4785 = PLANE ( 'NONE',  #18004 ) ;
#4786 = CARTESIAN_POINT ( 'NONE',  ( -12.71530858231679417, -23.77099543870833998, 2.825813738724734847 ) ) ;
#4787 = ADVANCED_FACE ( 'NONE', ( #9755 ), #16140, .F. ) ;
#4788 = LINE ( 'NONE', #10116, #6284 ) ;
#4789 = CARTESIAN_POINT ( 'NONE',  ( 8.503441417683177406, -22.05068747287766229, 6.000000000000001776 ) ) ;
#4790 =( LENGTH_UNIT ( ) NAMED_UNIT ( * ) SI_UNIT ( .MILLI., .METRE. ) );
#4791 = CARTESIAN_POINT ( 'NONE',  ( -5.409691417683178294, -21.32581373872474373, 5.270995438708348857 ) ) ;
#4792 = VECTOR ( 'NONE', #7210, 1000.000000000000000 ) ;
#4793 = VERTEX_POINT ( 'NONE', #14144 ) ;
#4794 = ADVANCED_BREP_SHAPE_REPRESENTATION ( '', ( #11472, #18039 ), #12033 ) ;
#4795 = CARTESIAN_POINT ( 'NONE',  ( 4.746558582316793284, -21.94931252712234482, 5.250000000000000888 ) ) ;
#4796 = CARTESIAN_POINT ( 'NONE',  ( -3.997260319564023501, 9.000000000000001776, 0.000000000000000000 ) ) ;
#4797 = CARTESIAN_POINT ( 'NONE',  ( -12.66144083004408571, -19.15973808277258073, 6.259475412489329038 ) ) ;
#4798 = ORIENTED_EDGE ( 'NONE', *, *, #4350, .F. ) ;
#4799 = CARTESIAN_POINT ( 'NONE',  ( 7.184058582316794173, -20.79840458871652942, 2.226721677130544030 ) ) ;
#4800 = EDGE_CURVE ( 'NONE', #9362, #6964, #20551, .T. ) ;
#4801 = CARTESIAN_POINT ( 'NONE',  ( 20.50349085826861995, 10.00000000000000000, 0.000000000000000000 ) ) ;
#4802 = ADVANCED_FACE ( 'NONE', ( #4626 ), #9546, .T. ) ;
#4803 = ORIENTED_EDGE ( 'NONE', *, *, #2928, .T. ) ;
#4804 = DIRECTION ( 'NONE',  ( 0.000000000000000000, -0.2487476929738665354, -0.9685683172808094987 ) ) ;
#4805 = DIRECTION ( 'NONE',  ( 1.000000000000000000, 0.000000000000000000, 0.000000000000000000 ) ) ;
#4806 = ORIENTED_EDGE ( 'NONE', *, *, #5623, .F. ) ;
#4807 = EDGE_CURVE ( 'NONE', #16861, #13083, #7877, .T. ) ;
#4808 = DIRECTION ( 'NONE',  ( -3.469446951953611033E-15, 1.000000000000000000, 0.000000000000000000 ) ) ;
#4809 = VERTEX_POINT ( 'NONE', #31 ) ;
#4810 = CARTESIAN_POINT ( 'NONE',  ( -6.434058582316794173, -23.20159541128345992, 4.773278322869455970 ) ) ;
#4811 = CARTESIAN_POINT ( 'NONE',  ( 12.64511805349267526, -19.23403829861753422, 5.507852591554869726 ) ) ;
#4812 = CARTESIAN_POINT ( 'NONE',  ( -9.999999999999998224, -30.00000000000000355, 1.000000000000000000 ) ) ;
#4813 = CARTESIAN_POINT ( 'NONE',  ( 1.733187991654075777, -9.867296153774269385, 1.623254759047128237 ) ) ;
#4814 = ADVANCED_FACE ( 'NONE', ( #6302 ), #343, .T. ) ;
#4815 =( BOUNDED_CURVE ( )  B_SPLINE_CURVE ( 3, ( #4512, #17474, #7760, #14126 ),
 .UNSPECIFIED., .F., .T. ) 
 B_SPLINE_CURVE_WITH_KNOTS ( ( 4, 4 ),
 ( 0.001187255941418635012, 0.002344578398797381343 ),
 .UNSPECIFIED. ) 
 CURVE ( )  GEOMETRIC_REPRESENTATION_ITEM ( )  RATIONAL_B_SPLINE_CURVE ( ( 0.9619191252709787809, 0.3335846922424358096, 0.3462783171521095493, 1.000000000000000000 ) ) 
 REPRESENTATION_ITEM ( '' )  );
#4816 = CARTESIAN_POINT ( 'NONE',  ( -26.04469207716614676, 4.999999999999999112, 1.000000000000000000 ) ) ;
#4817 = CARTESIAN_POINT ( 'NONE',  ( -13.42766088059286922, -16.84062553004338625, 4.794749963382423985 ) ) ;
#4818 = CARTESIAN_POINT ( 'NONE',  ( 9.621558582316794173, -23.74999999999999645, 3.550687472877651629 ) ) ;
#4819 = CARTESIAN_POINT ( 'NONE',  ( -13.88684657106908205, 4.848251838987907014, 6.535242036940271504 ) ) ;
#4820 = LINE ( 'NONE', #6089, #17067 ) ;
#4821 = CARTESIAN_POINT ( 'NONE',  ( -7.559058582316795949, -20.19639159124062999, 5.231925497173373074 ) ) ;
#4822 = CARTESIAN_POINT ( 'NONE',  ( 7.371558582316794173, -20.24999999999999289, 3.449312527122348371 ) ) ;
#4823 = CARTESIAN_POINT ( 'NONE',  ( 8.222191417683175629, -21.02099543870834353, 3.964901035250761208 ) ) ;
#4824 = CARTESIAN_POINT ( 'NONE',  ( -8.222191417683175629, -20.27099543870833998, 4.275561207030583510 ) ) ;
#4825 = ORIENTED_EDGE ( 'NONE', *, *, #11417, .F. ) ;
#4826 = CARTESIAN_POINT ( 'NONE',  ( 13.84402619238587206, 4.185822715484293077, 5.150938132831436533 ) ) ;
#4827 = CARTESIAN_POINT ( 'NONE',  ( -2.708677329869237482, -9.785633270066144362, 1.794897081886200230 ) ) ;
#4828 = EDGE_LOOP ( 'NONE', ( #7771, #1102, #3440, #16016 ) ) ;
#4829 = EDGE_LOOP ( 'NONE', ( #18627, #11636, #8292, #1819 ) ) ;
#4830 = CARTESIAN_POINT ( 'NONE',  ( 17.30017143803810242, 4.999999999999999112, 1.000000000000000000 ) ) ;
#4831 = DIRECTION ( 'NONE',  ( 1.000000000000000000, 0.000000000000000000, -0.000000000000000000 ) ) ;
#4832 = CARTESIAN_POINT ( 'NONE',  ( 4.999999999999998224, -7.500000000000047073, 9.999999999999998224 ) ) ;
#4833 = CARTESIAN_POINT ( 'NONE',  ( -3.270401025279431995, -9.547343748290430199, 2.676314555138040063 ) ) ;
#4834 = CARTESIAN_POINT ( 'NONE',  ( 0.000000000000000000, 4.999999999999999112, 1.000000000000000000 ) ) ;
#4835 = EDGE_CURVE ( 'NONE', #2170, #13899, #5049, .T. ) ;
#4836 = DIRECTION ( 'NONE',  ( 0.000000000000000000, -0.2487476929738665354, -0.9685683172808094987 ) ) ;
#4837 = CARTESIAN_POINT ( 'NONE',  ( -12.83635126708105823, -9.576761012430582198, 5.715524842913705328 ) ) ;
#4838 = CARTESIAN_POINT ( 'NONE',  ( 11.77780858231679773, -20.27099543870833642, 2.724438792969431589 ) ) ;
#4839 = DIRECTION ( 'NONE',  ( -0.000000000000000000, -0.000000000000000000, -1.000000000000000000 ) ) ;
#4840 = CARTESIAN_POINT ( 'NONE',  ( 13.15498530132288479, 5.764257716805535559, 3.666666666666500873 ) ) ;
#4841 = CARTESIAN_POINT ( 'NONE',  ( -1.903957340438703572, -10.27085516675799148, 2.476896775482616331 ) ) ;
#4842 = ORIENTED_EDGE ( 'NONE', *, *, #18197, .F. ) ;
#4843 = CARTESIAN_POINT ( 'NONE',  ( -13.39722611581222189, -19.12758115148224647, 5.495601574623241170 ) ) ;
#4844 = LINE ( 'NONE', #14462, #7721 ) ;
#4845 = CARTESIAN_POINT ( 'NONE',  ( 5.690941417683177406, -23.80360840875937001, 5.231925497173365081 ) ) ;
#4846 = CARTESIAN_POINT ( 'NONE',  ( -12.90280858231679595, -22.46490103525074034, 2.520995438708341307 ) ) ;
#4847 = VERTEX_POINT ( 'NONE', #10068 ) ;
#4848 = CARTESIAN_POINT ( 'NONE',  ( 12.62500028073152869, -20.99998582305707728, 4.544498183892649479 ) ) ;
#4849 = CARTESIAN_POINT ( 'NONE',  ( 12.62499999999998401, -19.49999999999998934, 3.146526952850934755 ) ) ;
#4850 = CARTESIAN_POINT ( 'NONE',  ( 8.119520639128047890, 0.000000000000000000, 1.000000000000000000 ) ) ;
#4851 = VERTEX_POINT ( 'NONE', #14663 ) ;
#4852 = ORIENTED_EDGE ( 'NONE', *, *, #409, .F. ) ;
#4853 = CARTESIAN_POINT ( 'NONE',  ( -5.933390479346035029, 4.999999999999999112, 1.000000000000000000 ) ) ;
#4854 = COLOUR_RGB ( '', 0.09019608, 0.27058824, 0.51372549) ;
#4855 = CARTESIAN_POINT ( 'NONE',  ( 15.00000000000000000, 0.000000000000000000, 1.000000000000000000 ) ) ;
#4856 = EDGE_LOOP ( 'NONE', ( #18927, #4421, #1553, #14880, #11258, #15418, #2587, #11256 ) ) ;
#4857 = DIRECTION ( 'NONE',  ( 1.000000000000000000, 0.000000000000000000, 0.000000000000000000 ) ) ;
#4858 = CARTESIAN_POINT ( 'NONE',  ( 2.557403344953185442, -14.91030650174552896, 3.668400560659690779 ) ) ;
#4859 = DIRECTION ( 'NONE',  ( 1.000000000000000000, 0.000000000000000000, -0.000000000000000000 ) ) ;
#4860 = CARTESIAN_POINT ( 'NONE',  ( 7.499999999999999112, -18.49999999999999645, 6.500000000000000888 ) ) ;
#4861 = ADVANCED_FACE ( 'NONE', ( #2013, #3886 ), #16538, .T. ) ;
#4862 = LINE ( 'NONE', #12707, #6016 ) ;
#4863 = CARTESIAN_POINT ( 'NONE',  ( -14.49999999999998579, -21.99999999999999645, 14.18378559369222280 ) ) ;
#4864 = CARTESIAN_POINT ( 'NONE',  ( -12.90280858231679773, -22.77556120703056308, 1.770995438708339975 ) ) ;
#4865 = CARTESIAN_POINT ( 'NONE',  ( -13.37327929115833491, -20.24999999560066399, 3.449077790995343840 ) ) ;
#4866 = VECTOR ( 'NONE', #11989, 1000.000000000000000 ) ;
#4867 = CARTESIAN_POINT ( 'NONE',  ( 10.09030858231679595, -21.63647391050454871, 2.479004561291657804 ) ) ;
#4868 = CARTESIAN_POINT ( 'NONE',  ( -12.62562661273123332, -19.46835605706984040, 4.628101975944573176 ) ) ;
#4869 = CARTESIAN_POINT ( 'NONE',  ( -5.777808582316795949, -21.02099543870833998, 3.035098964749253003 ) ) ;
#4870 = CARTESIAN_POINT ( 'NONE',  ( -11.69094141768317563, -23.27327832286946219, 4.701595411283453707 ) ) ;
#4871 = VERTEX_POINT ( 'NONE', #11426 ) ;
#4872 = EDGE_CURVE ( 'NONE', #11469, #18418, #2313, .T. ) ;
#4873 = CARTESIAN_POINT ( 'NONE',  ( 13.81612658856640863, 2.776892722604777930, 5.216624963382545666 ) ) ;
#4874 = VERTEX_POINT ( 'NONE', #14769 ) ;
#4875 = EDGE_CURVE ( 'NONE', #20379, #10445, #11733, .T. ) ;
#4876 = ORIENTED_EDGE ( 'NONE', *, *, #16737, .F. ) ;
#4877 = CARTESIAN_POINT ( 'NONE',  ( 0.000000000000000000, 16.00000000000000000, 1.000000000000000000 ) ) ;
#4878 = EDGE_LOOP ( 'NONE', ( #19781, #10248 ) ) ;
#4879 = PLANE ( 'NONE',  #6767 ) ;
#4880 = ORIENTED_EDGE ( 'NONE', *, *, #2536, .T. ) ;
#4881 = CARTESIAN_POINT ( 'NONE',  ( 9.065941417683177406, -23.20159541128344927, 2.226721677130534705 ) ) ;
#4882 = DIRECTION ( 'NONE',  ( -0.000000000000000000, -0.000000000000000000, -1.000000000000000000 ) ) ;
#4883 = CARTESIAN_POINT ( 'NONE',  ( -1.655860418491166941, -9.114909740826840689, 2.372641880528837621 ) ) ;
#4884 = CARTESIAN_POINT ( 'NONE',  ( 2.602174906157317835, -9.976397331638239052, 2.593889103792902606 ) ) ;
#4885 = LINE ( 'NONE', #3122, #17981 ) ;
#4886 = EDGE_CURVE ( 'NONE', #8434, #16176, #13401, .T. ) ;
#4887 = CARTESIAN_POINT ( 'NONE',  ( 8.784691417683177406, -23.77099543870834353, 4.174186261275252718 ) ) ;
#4888 = CARTESIAN_POINT ( 'NONE',  ( -15.87779268661489773, 10.00000000000000000, 0.000000000000000000 ) ) ;
#4889 = CARTESIAN_POINT ( 'NONE',  ( -11.78469141768317741, -23.02099543870834353, 3.863526089495429972 ) ) ;
#4890 = ORIENTED_EDGE ( 'NONE', *, *, #15799, .T. ) ;
#4891 = CARTESIAN_POINT ( 'NONE',  ( 7.277808582316795061, -19.52099543870833642, 2.413778621189609286 ) ) ;
#4892 = EDGE_CURVE ( 'NONE', #9041, #10100, #9954, .T. ) ;
#4893 = PLANE ( 'NONE',  #4736 ) ;
#4894 = CARTESIAN_POINT ( 'NONE',  ( -12.62499999999998224, -21.00000000000006395, 4.416666666666682062 ) ) ;
#4895 = ORIENTED_EDGE ( 'NONE', *, *, #9073, .F. ) ;
#4896 = ADVANCED_FACE ( 'NONE', ( #18125 ), #446, .T. ) ;
#4897 = FACE_OUTER_BOUND ( 'NONE', #7017, .T. ) ;
#4898 = CARTESIAN_POINT ( 'NONE',  ( -13.67791111847408025, 9.000000000000001776, 1.000000000000000000 ) ) ;
#4899 = ORIENTED_EDGE ( 'NONE', *, *, #566, .T. ) ;
#4900 = CARTESIAN_POINT ( 'NONE',  ( -5.563547257480587760, 10.00000000000000000, 1.000000000000000000 ) ) ;
#4901 = CARTESIAN_POINT ( 'NONE',  ( 2.324238743289460347E-16, 5.000000000000047962, 1.000000000000000000 ) ) ;
#4902 = VERTEX_POINT ( 'NONE', #16633 ) ;
#4903 = ADVANCED_FACE ( 'NONE', ( #6825 ), #8703, .T. ) ;
#4904 = DIRECTION ( 'NONE',  ( 1.000000000000000000, 0.000000000000000000, 0.000000000000000000 ) ) ;
#4905 = ORIENTED_EDGE ( 'NONE', *, *, #2896, .F. ) ;
#4906 = CARTESIAN_POINT ( 'NONE',  ( -12.34030858231679773, -22.98484643305508612, 6.020995438708344416 ) ) ;
#4907 = DIRECTION ( 'NONE',  ( -0.000000000000000000, -0.000000000000000000, -1.000000000000000000 ) ) ;
#4908 = DIRECTION ( 'NONE',  ( -0.000000000000000000, 1.000000000000000000, -0.000000000000000000 ) ) ;
#4909 = CARTESIAN_POINT ( 'NONE',  ( 1.963707630584672570, -9.980492102769451535, 1.652325740065381909 ) ) ;
#4910 = EDGE_CURVE ( 'NONE', #2930, #3253, #6619, .T. ) ;
#4911 = CARTESIAN_POINT ( 'NONE',  ( 12.66369984131459070, -18.29565801360988075, 5.528024842915327142 ) ) ;
#4912 = EDGE_CURVE ( 'NONE', #14572, #13516, #5149, .T. ) ;
#4913 = DIRECTION ( 'NONE',  ( -0.000000000000000000, -1.000000000000000000, -0.000000000000000000 ) ) ;
#4914 = CARTESIAN_POINT ( 'NONE',  ( -13.79214722387705905, 1.565934805775630601, 5.190583296715636230 ) ) ;
#4915 = CARTESIAN_POINT ( 'NONE',  ( 5.402808582316794173, -22.77556120703056308, 1.770995438708339975 ) ) ;
#4916 = CARTESIAN_POINT ( 'NONE',  ( -12.66863463945108137, -18.79645070772368953, 6.267287912489321045 ) ) ;
#4917 = CARTESIAN_POINT ( 'NONE',  ( 27.00000000000000000, 3.000000000000000000, 1.000000000000000000 ) ) ;
#4918 = CARTESIAN_POINT ( 'NONE',  ( -9.059058582316795949, -20.19639159124062999, 5.231925497173373074 ) ) ;
#4919 = CARTESIAN_POINT ( 'NONE',  ( 4.934058582316793284, -23.20159541128345992, 4.773278322869455970 ) ) ;
#4920 = CARTESIAN_POINT ( 'NONE',  ( 5.972191417683178294, -22.97900456129165292, 3.035098964749240125 ) ) ;
#4921 = CARTESIAN_POINT ( 'NONE',  ( -6.347191417683176518, -21.22443879296941915, 1.770995438708345748 ) ) ;
#4922 = ORIENTED_EDGE ( 'NONE', *, *, #6382, .T. ) ;
#4923 = ORIENTED_EDGE ( 'NONE', *, *, #9382, .T. ) ;
#4924 = CARTESIAN_POINT ( 'NONE',  ( 13.84501469867365131, 4.235742283194553259, 3.333333333332063386 ) ) ;
#4925 = AXIS2_PLACEMENT_3D ( 'NONE', #11285, #6270, #15687 ) ;
#4926 = DIRECTION ( 'NONE',  ( -0.000000000000000000, 0.000000000000000000, -1.000000000000000000 ) ) ;
#4927 = LINE ( 'NONE', #328, #9348 ) ;
#4928 = VERTEX_POINT ( 'NONE', #11527 ) ;
#4929 = VERTEX_POINT ( 'NONE', #13291 ) ;
#4930 = CARTESIAN_POINT ( 'NONE',  ( -5.933390479346035029, 4.999999999999999112, 0.000000000000000000 ) ) ;
#4931 = DIRECTION ( 'NONE',  ( -1.000000000000000000, 0.000000000000000000, -0.000000000000000000 ) ) ;
#4932 = CARTESIAN_POINT ( 'NONE',  ( 13.37327929115833669, -20.24999999707183207, 3.449077790995325632 ) ) ;
#4933 = CARTESIAN_POINT ( 'NONE',  ( -1.643076795806035717, -8.364903549957356077, 2.372640290589878909 ) ) ;
#4934 = CARTESIAN_POINT ( 'NONE',  ( 4.000000000000000000, -12.50000000000000000, 1.000000000000000000 ) ) ;
#4935 = EDGE_CURVE ( 'NONE', #18601, #15348, #20440, .T. ) ;
#4936 = EDGE_CURVE ( 'NONE', #11456, #9694, #11623, .T. ) ;
#4937 = CARTESIAN_POINT ( 'NONE',  ( -27.94203811574922725, 3.231447299068595019E-14, 0.000000000000000000 ) ) ;
#4938 = CARTESIAN_POINT ( 'NONE',  ( -12.62503117662529739, -20.24842558042254836, 4.565011198945062354 ) ) ;
#4939 = DIRECTION ( 'NONE',  ( -0.000000000000000000, -0.000000000000000000, -1.000000000000000000 ) ) ;
#4940 = LINE ( 'NONE', #6521, #387 ) ;
#4941 = CARTESIAN_POINT ( 'NONE',  ( 13.13728495444130751, 4.870390199291127153, 6.548325014280736767 ) ) ;
#4942 = CARTESIAN_POINT ( 'NONE',  ( -1.776440835594205847, -9.874406767442327038, 1.625080906685880233 ) ) ;
#4943 = ORIENTED_EDGE ( 'NONE', *, *, #14069, .T. ) ;
#4944 = CARTESIAN_POINT ( 'NONE',  ( -13.87470586348985258, 4.985146106231644225, 5.033049509202228933 ) ) ;
#4945 = CARTESIAN_POINT ( 'NONE',  ( -13.49999999999998401, -25.49999999999999645, 4.000000000000000000 ) ) ;
#4946 = AXIS2_PLACEMENT_3D ( 'NONE', #11382, #11683, #3748 ) ;
#4947 = CARTESIAN_POINT ( 'NONE',  ( 4.378441417683176518, -24.50000000000000000, 3.449312527122335048 ) ) ;
#4948 = CARTESIAN_POINT ( 'NONE',  ( -6.996558582316795949, -22.05068747287764452, 2.499999999999999112 ) ) ;
#4949 = ORIENTED_EDGE ( 'NONE', *, *, #6104, .T. ) ;
#4950 = CARTESIAN_POINT ( 'NONE',  ( 12.63178515739782348, -20.65734955141111584, 5.567013446834313761 ) ) ;
#4951 = CARTESIAN_POINT ( 'NONE',  ( 13.05696142222617695, 1.564051822406025583, 5.955108176248398166 ) ) ;
#4952 = CARTESIAN_POINT ( 'NONE',  ( -3.997260319564023501, 9.000000000000001776, 1.000000000000000000 ) ) ;
#4953 = ORIENTED_EDGE ( 'NONE', *, *, #10552, .F. ) ;
#4954 = EDGE_CURVE ( 'NONE', #8157, #7916, #8498, .T. ) ;
#4955 = ORIENTED_EDGE ( 'NONE', *, *, #5239, .T. ) ;
#4956 = DIRECTION ( 'NONE',  ( 1.000000000000000000, 0.000000000000000000, 0.000000000000000000 ) ) ;
#4957 = CLOSED_SHELL ( 'NONE', ( #4426, #8724, #15599, #4802, #15798, #5412, #4632, #19562, #12719, #530, #8440, #6806, #383, #10255, #459, #10301, #16890, #7051, #17076, #9542, #20019, #8582, #10441, #831, #16791, #5261, #5051, #13923, #2108, #16643, #20503, #17154, #11687, #16299, #4253, #19070, #3423, #6179, #19588, #19597, #7308, #12742, #12322, #7848, #9423, #7126, #8404, #3449, #6150, #16964, #16043, #8605, #8840 ) ) ;
#4958 = CARTESIAN_POINT ( 'NONE',  ( -24.79469207716615031, 9.000000000000001776, 1.000000000000000000 ) ) ;
#4959 =( GEOMETRIC_REPRESENTATION_CONTEXT ( 3 ) GLOBAL_UNCERTAINTY_ASSIGNED_CONTEXT ( ( #8824 ) ) GLOBAL_UNIT_ASSIGNED_CONTEXT ( ( #16287, #13147, #5198 ) ) REPRESENTATION_CONTEXT ( 'NONE', 'WORKASPACE' ) );
#4960 = LINE ( 'NONE', #8307, #12311 ) ;
#4961 = LINE ( 'NONE', #11340, #10001 ) ;
#4962 = CARTESIAN_POINT ( 'NONE',  ( 1.872293763630120678, -10.04602735435188698, 2.419156501869924369 ) ) ;
#4963 = CARTESIAN_POINT ( 'NONE',  ( -25.29469207716615031, 0.000000000000000000, 1.000000000000000000 ) ) ;
#4964 = DIRECTION ( 'NONE',  ( -0.000000000000000000, -0.000000000000000000, -1.000000000000000000 ) ) ;
#4965 = CARTESIAN_POINT ( 'NONE',  ( -13.50000000000000178, 5.000000000000047962, 2.000000000000000000 ) ) ;
#4966 = CARTESIAN_POINT ( 'NONE',  ( -7.869520639128047002, 4.999999999999999112, 1.000000000000000000 ) ) ;
#4967 = CARTESIAN_POINT ( 'NONE',  ( 15.06494360078803041, 10.00000000000000000, 1.000000000000000000 ) ) ;
#4968 = CARTESIAN_POINT ( 'NONE',  ( -12.90248710081030481, -20.62497818207526024, 3.513302565646801323 ) ) ;
#4969 = AXIS2_PLACEMENT_3D ( 'NONE', #19636, #15222, #5607 ) ;
#4970 = CIRCLE ( 'NONE', #15639, 0.3749999999999997224 ) ;
#4971 = CARTESIAN_POINT ( 'NONE',  ( -13.09533517714100093, 4.251926445620864747, 5.084080158857392284 ) ) ;
#4972 = CARTESIAN_POINT ( 'NONE',  ( -6.152808582316795949, -21.53509896474924901, 4.479004561291659137 ) ) ;
#4973 = CARTESIAN_POINT ( 'NONE',  ( -5.034691417683178294, -20.22900456129164581, 2.825813738724747726 ) ) ;
#4974 = VECTOR ( 'NONE', #10402, 1000.000000000000000 ) ;
#4975 = VERTEX_POINT ( 'NONE', #8595 ) ;
#4976 = CARTESIAN_POINT ( 'NONE',  ( 13.45643611822145225, -15.38747602984844853, 4.825999963382285429 ) ) ;
#4977 = CARTESIAN_POINT ( 'NONE',  ( -16.62779268661489951, 0.000000000000000000, 0.000000000000000000 ) ) ;
#4978 = ORIENTED_EDGE ( 'NONE', *, *, #13856, .T. ) ;
#4979 = VERTEX_POINT ( 'NONE', #646 ) ;
#4980 = LINE ( 'NONE', #16076, #18086 ) ;
#4981 = VERTEX_POINT ( 'NONE', #543 ) ;
#4982 = CARTESIAN_POINT ( 'NONE',  ( 24.62918902992234038, 11.64110105645932691, 0.000000000000000000 ) ) ;
#4983 = EDGE_CURVE ( 'NONE', #8074, #999, #18224, .T. ) ;
#4984 = VECTOR ( 'NONE', #4857, 1000.000000000000000 ) ;
#4985 = ORIENTED_EDGE ( 'NONE', *, *, #9443, .F. ) ;
#4986 = CARTESIAN_POINT ( 'NONE',  ( 8.409691417683177406, -21.32581373872474373, 5.270995438708348857 ) ) ;
#4987 = DIRECTION ( 'NONE',  ( -0.000000000000000000, -0.000000000000000000, -1.000000000000000000 ) ) ;
#4988 = VECTOR ( 'NONE', #11997, 1000.000000000000000 ) ;
#4989 = CARTESIAN_POINT ( 'NONE',  ( -25.29469207716615031, 9.000000000000001776, 1.000000000000000000 ) ) ;
#4990 = CARTESIAN_POINT ( 'NONE',  ( 2.513306525444908512, -9.622685169956881168, 2.503048754562789746 ) ) ;
#4991 = DIRECTION ( 'NONE',  ( 1.000000000000000000, 0.000000000000000000, 0.000000000000000000 ) ) ;
#4992 = EDGE_CURVE ( 'NONE', #14620, #4337, #19692, .T. ) ;
#4993 = CARTESIAN_POINT ( 'NONE',  ( 7.940941417683176518, -20.72672167713052715, 2.298404588716546293 ) ) ;
#4994 = CARTESIAN_POINT ( 'NONE',  ( -14.49999999999998579, -18.49999999999999645, 4.000000000000000000 ) ) ;
#4995 = CARTESIAN_POINT ( 'NONE',  ( -10.37844141768317741, -22.99999999999999645, 3.449312527122335048 ) ) ;
#4996 = VERTEX_POINT ( 'NONE', #18434 ) ;
#4997 = CARTESIAN_POINT ( 'NONE',  ( 9.809058582316795949, -23.80360840875935935, 1.768074502826626260 ) ) ;
#4998 = CARTESIAN_POINT ( 'NONE',  ( 12.62888984277510218, -20.05356293986039873, 5.111704976569332537 ) ) ;
#4999 = CARTESIAN_POINT ( 'NONE',  ( -13.12405442816082868, 4.202248622120948518, 6.747400073346936367 ) ) ;
#5000 = ORIENTED_EDGE ( 'NONE', *, *, #2432, .T. ) ;
#5001 = CARTESIAN_POINT ( 'NONE',  ( 21.25349085826861995, 10.00000000000000000, 1.000000000000000000 ) ) ;
#5002 = FACE_OUTER_BOUND ( 'NONE', #7682, .T. ) ;
#5003 = VECTOR ( 'NONE', #14156, 1000.000000000000000 ) ;
#5004 = ORIENTED_EDGE ( 'NONE', *, *, #11635, .T. ) ;
#5005 = PRODUCT_DEFINITION_SHAPE ( 'NONE', 'NONE',  #19177 ) ;
#5006 = DIRECTION ( 'NONE',  ( 0.000000000000000000, 0.000000000000000000, 1.000000000000000000 ) ) ;
#5007 = VERTEX_POINT ( 'NONE', #954 ) ;
#5008 = VECTOR ( 'NONE', #7644, 1000.000000000000000 ) ;
#5009 = EDGE_CURVE ( 'NONE', #5007, #16377, #13811, .T. ) ;
#5010 = CARTESIAN_POINT ( 'NONE',  ( 13.28675616151867267, -20.00825975431586912, 3.460912183795370023 ) ) ;
#5011 = EDGE_LOOP ( 'NONE', ( #7940, #8254, #7686, #4923 ) ) ;
#5012 = CARTESIAN_POINT ( 'NONE',  ( -7.090308582316794173, -21.32581373872472597, 1.729004561291657582 ) ) ;
#5013 = FACE_OUTER_BOUND ( 'NONE', #18208, .T. ) ;
#5014 = LINE ( 'NONE', #4812, #5121 ) ;
#5015 = CARTESIAN_POINT ( 'NONE',  ( 1.513434189748285918, -9.864917468222230923, 1.622643865078341907 ) ) ;
#5016 = EDGE_CURVE ( 'NONE', #12491, #8181, #2625, .T. ) ;
#5017 = CARTESIAN_POINT ( 'NONE',  ( 13.08094078691552831, 2.775009739235173356, 5.981149842915306714 ) ) ;
#5018 = LINE ( 'NONE', #18196, #14021 ) ;
#5019 = CARTESIAN_POINT ( 'NONE',  ( -13.84501469867711698, 4.235742283194553259, 4.583333333333295734 ) ) ;
#5020 = CARTESIAN_POINT ( 'NONE',  ( 12.99655858231679595, -22.05068747287764452, 0.9999999999999978906 ) ) ;
#5021 = CARTESIAN_POINT ( 'NONE',  ( -13.15316049959406364, 5.672105229501871904, 5.573635960501007958 ) ) ;
#5022 = CARTESIAN_POINT ( 'NONE',  ( -12.62844141768317741, -19.49999999999998934, 3.550687472877664952 ) ) ;
#5023 = VECTOR ( 'NONE', #13696, 1000.000000000000000 ) ;
#5024 = PLANE ( 'NONE',  #3706 ) ;
#5025 = CARTESIAN_POINT ( 'NONE',  ( 4.315753587183822404, -21.47141115243053378, 5.558207674221720573 ) ) ;
#5026 = CARTESIAN_POINT ( 'NONE',  ( 9.527808582316795949, -22.97900456129165647, 3.964901035250747885 ) ) ;
#5027 = CARTESIAN_POINT ( 'NONE',  ( -5.597191417683177406, -22.77556120703057729, 5.229004561291656472 ) ) ;
#5028 = ORIENTED_EDGE ( 'NONE', *, *, #6218, .T. ) ;
#5029 = VERTEX_POINT ( 'NONE', #12040 ) ;
#5030 = CARTESIAN_POINT ( 'NONE',  ( 13.37503071710846925, -20.24844878602346299, 4.564052989354591361 ) ) ;
#5031 = CARTESIAN_POINT ( 'NONE',  ( 13.92791111847407848, 4.999999999999999112, 0.000000000000000000 ) ) ;
#5032 = CARTESIAN_POINT ( 'NONE',  ( -15.00000000000000000, -6.000000000000000000, 1.000000000000000000 ) ) ;
#5033 = EDGE_LOOP ( 'NONE', ( #15136, #18546, #3025, #7583 ) ) ;
#5034 = EDGE_CURVE ( 'NONE', #17531, #16862, #10795, .T. ) ;
#5035 = PRODUCT_DEFINITION_FORMATION_WITH_SPECIFIED_SOURCE ( 'ANY', '', #19212, .NOT_KNOWN. ) ;
#5036 = VERTEX_POINT ( 'NONE', #17163 ) ;
#5037 = CYLINDRICAL_SURFACE ( 'NONE', #4099, 10.00000000000000000 ) ;
#5038 = CIRCLE ( 'NONE', #11701, 0.4999999999999987232 ) ;
#5039 = CARTESIAN_POINT ( 'NONE',  ( -22.06633994409548194, 11.64110105645932691, 10.00000000000000000 ) ) ;
#5040 = VECTOR ( 'NONE', #16476, 1000.000000000000000 ) ;
#5041 = AXIS2_PLACEMENT_3D ( 'NONE', #20165, #17111, #2793 ) ;
#5042 = CARTESIAN_POINT ( 'NONE',  ( -13.11145189917479392, 4.315820908324673688, 5.961432613039677086 ) ) ;
#5043 = VECTOR ( 'NONE', #7031, 1000.000000000000000 ) ;
#5044 = FACE_OUTER_BOUND ( 'NONE', #5011, .T. ) ;
#5045 = CARTESIAN_POINT ( 'NONE',  ( -2.801385037117921861, -10.23463596792102415, 1.910209944425432349 ) ) ;
#5046 = DIRECTION ( 'NONE',  ( -1.000000000000000000, -0.000000000000000000, -0.000000000000000000 ) ) ;
#5047 = CARTESIAN_POINT ( 'NONE',  ( -13.12463908936614132, 4.981774012991869505, 5.264611377988129171 ) ) ;
#5048 = SURFACE_SIDE_STYLE ('',( #19390 ) ) ;
#5049 = LINE ( 'NONE', #16339, #17070 ) ;
#5050 = CARTESIAN_POINT ( 'NONE',  ( 12.64195242771744709, -19.39390240027112000, 5.496549442168085164 ) ) ;
#5051 = ADVANCED_FACE ( 'NONE', ( #15180 ), #20004, .T. ) ;
#5052 = CARTESIAN_POINT ( 'NONE',  ( -1.513434189748285918, -9.864917468222230923, 2.372643865078341019 ) ) ;
#5053 = ORIENTED_EDGE ( 'NONE', *, *, #17145, .F. ) ;
#5054 = CARTESIAN_POINT ( 'NONE',  ( -13.44218742460511073, -16.85703505742523234, 5.544429699623282914 ) ) ;
#5055 = DIRECTION ( 'NONE',  ( 1.000000000000000000, 0.000000000000000000, 0.000000000000000000 ) ) ;
#5056 = VECTOR ( 'NONE', #19827, 1000.000000000000000 ) ;
#5057 = CARTESIAN_POINT ( 'NONE',  ( 6.628441417683177406, -19.49999999999998934, 3.550687472877664952 ) ) ;
#5058 = CARTESIAN_POINT ( 'NONE',  ( -5.402808582316795949, -22.46490103525074034, 2.520995438708341307 ) ) ;
#5059 = ORIENTED_EDGE ( 'NONE', *, *, #14111, .F. ) ;
#5060 = CARTESIAN_POINT ( 'NONE',  ( 13.90439735423812273, 5.734566389025032684, 4.666666666666618113 ) ) ;
#5061 = CARTESIAN_POINT ( 'NONE',  ( 12.65410809543883985, -18.78004118034163739, 5.517608176248461227 ) ) ;
#5062 = PLANE ( 'NONE',  #12667 ) ;
#5063 = ORIENTED_EDGE ( 'NONE', *, *, #10818, .T. ) ;
#5064 = EDGE_CURVE ( 'NONE', #7837, #965, #1169, .T. ) ;
#5065 = EDGE_LOOP ( 'NONE', ( #19511, #11358, #4124, #12971 ) ) ;
#5066 = ADVANCED_FACE ( 'NONE', ( #18326 ), #7448, .T. ) ;
#5067 = LINE ( 'NONE', #11138, #19463 ) ;
#5068 = PLANE ( 'NONE',  #14894 ) ;
#5069 = DIRECTION ( 'NONE',  ( 1.000000000000000000, 0.000000000000000000, 0.000000000000000000 ) ) ;
#5070 = VECTOR ( 'NONE', #2400, 1000.000000000000000 ) ;
#5071 = CARTESIAN_POINT ( 'NONE',  ( 13.87470602645761808, 4.985154336109792972, 4.000000000000000000 ) ) ;
#5072 = CARTESIAN_POINT ( 'NONE',  ( 1.407845757905374695, -9.864917468222230923, 1.622643865078341907 ) ) ;
#5073 = CARTESIAN_POINT ( 'NONE',  ( 3.499999999999998668, -24.49999999999999289, 1.000000000000000000 ) ) ;
#5074 = DIRECTION ( 'NONE',  ( 0.000000000000000000, -1.000000000000000000, 0.000000000000000000 ) ) ;
#5075 = ADVANCED_FACE ( 'NONE', ( #9117 ), #19799, .F. ) ;
#5076 = FACE_OUTER_BOUND ( 'NONE', #2272, .T. ) ;
#5077 = DIRECTION ( 'NONE',  ( -1.000000000000000000, -2.312964634635730039E-15, 0.000000000000000000 ) ) ;
#5078 = DIRECTION ( 'NONE',  ( 1.000000000000000000, 0.000000000000000000, 0.000000000000000000 ) ) ;
#5079 = CARTESIAN_POINT ( 'NONE',  ( -2.616536356806028696, -10.07836329504444706, 2.620076000170431296 ) ) ;
#5080 = EDGE_LOOP ( 'NONE', ( #10676, #5283, #16588, #4520 ) ) ;
#5081 = CARTESIAN_POINT ( 'NONE',  ( -13.09001666039658573, 3.983341349998239966, 5.257104358157307367 ) ) ;
#5082 = CARTESIAN_POINT ( 'NONE',  ( -4.746558582316795061, -21.94931252712234127, 4.499999999999999112 ) ) ;
#5083 = CARTESIAN_POINT ( 'NONE',  ( -10.00344141768317563, -22.05068747287765873, 5.250000000000000888 ) ) ;
#5084 = ORIENTED_EDGE ( 'NONE', *, *, #7502, .T. ) ;
#5085 = CARTESIAN_POINT ( 'NONE',  ( 13.84501465882535598, 4.235740270674679842, 5.020612255068622076 ) ) ;
#5086 = CARTESIAN_POINT ( 'NONE',  ( -7.500000000000000888, -9.999999999999992895, 2.000000000000000000 ) ) ;
#5087 = ORIENTED_EDGE ( 'NONE', *, *, #16692, .F. ) ;
#5088 = ORIENTED_EDGE ( 'NONE', *, *, #197, .F. ) ;
#5089 = AXIS2_PLACEMENT_3D ( 'NONE', #11062, #15958, #19536 ) ;
#5090 = DIRECTION ( 'NONE',  ( 0.000000000000000000, -1.000000000000000000, 0.000000000000000000 ) ) ;
#5091 = ORIENTED_EDGE ( 'NONE', *, *, #5357, .F. ) ;
#5092 = CARTESIAN_POINT ( 'NONE',  ( 0.000000000000000000, 10.00000000000000000, 1.000000000000000000 ) ) ;
#5093 = VERTEX_POINT ( 'NONE', #17368 ) ;
#5094 = CARTESIAN_POINT ( 'NONE',  ( 5.128441417683177406, -20.24999999999999289, 3.550687472877664952 ) ) ;
#5095 = CARTESIAN_POINT ( 'NONE',  ( 10.05565079891005631, 9.000000000000001776, 0.000000000000000000 ) ) ;
#5096 = CARTESIAN_POINT ( 'NONE',  ( -1.837882866761050282, -9.938290523052360825, 2.391487531332776140 ) ) ;
#5097 = DIRECTION ( 'NONE',  ( 1.000000000000000000, 0.000000000000000000, 0.000000000000000000 ) ) ;
#5098 = CARTESIAN_POINT ( 'NONE',  ( -10.74655858231679417, -21.94931252712234482, 5.250000000000000888 ) ) ;
#5099 = VECTOR ( 'NONE', #19379, 1000.000000000000000 ) ;
#5100 = EDGE_CURVE ( 'NONE', #20584, #18396, #3055, .T. ) ;
#5101 =( NAMED_UNIT ( * ) PLANE_ANGLE_UNIT ( ) SI_UNIT ( $, .RADIAN. ) );
#5102 = CARTESIAN_POINT ( 'NONE',  ( 6.722191417683177406, -20.27099543870833998, 4.275561207030583510 ) ) ;
#5103 = FACE_OUTER_BOUND ( 'NONE', #18915, .T. ) ;
#5104 = CARTESIAN_POINT ( 'NONE',  ( -11.22219141768317741, -21.02099543870834353, 3.964901035250761208 ) ) ;
#5105 = ORIENTED_EDGE ( 'NONE', *, *, #11297, .F. ) ;
#5106 = CARTESIAN_POINT ( 'NONE',  ( 11.21530858231679595, -24.52099543870834708, 2.515153566944913432 ) ) ;
#5107 = CARTESIAN_POINT ( 'NONE',  ( 12.66369984131459070, -18.29565801360988075, 5.528024842915327142 ) ) ;
#5108 = CARTESIAN_POINT ( 'NONE',  ( -13.12519991495504712, 4.260095705229160146, 6.739971950528219402 ) ) ;
#5109 = ORIENTED_EDGE ( 'NONE', *, *, #3340, .F. ) ;
#5110 = LINE ( 'NONE', #11587, #2269 ) ;
#5111 = CARTESIAN_POINT ( 'NONE',  ( 0.000000000000000000, 4.999999999999999112, 1.000000000000000000 ) ) ;
#5112 = VECTOR ( 'NONE', #18920, 1000.000000000000000 ) ;
#5113 = ORIENTED_EDGE ( 'NONE', *, *, #12618, .F. ) ;
#5114 = ORIENTED_EDGE ( 'NONE', *, *, #3747, .T. ) ;
#5115 = AXIS2_PLACEMENT_3D ( 'NONE', #8802, #8900, #15170 ) ;
#5116 = CARTESIAN_POINT ( 'NONE',  ( -20.00349085826861995, 10.00000000000000000, 1.000000000000000000 ) ) ;
#5117 = EDGE_LOOP ( 'NONE', ( #2770, #14549, #1257, #6077 ) ) ;
#5118 = CARTESIAN_POINT ( 'NONE',  ( -11.49655858231679595, -22.05068747287764452, 0.9999999999999978906 ) ) ;
#5119 = CARTESIAN_POINT ( 'NONE',  ( 13.09293046926041626, 3.380488697651010011, 5.994170676248444352 ) ) ;
#5120 = FACE_OUTER_BOUND ( 'NONE', #8997, .T. ) ;
#5121 = VECTOR ( 'NONE', #14424, 1000.000000000000000 ) ;
#5122 = CARTESIAN_POINT ( 'NONE',  ( 12.83635126708105823, -9.576761012430582198, 5.715524842913705328 ) ) ;
#5123 = DIRECTION ( 'NONE',  ( -1.000000000000000000, 0.000000000000000000, 0.000000000000000000 ) ) ;
#5124 = CARTESIAN_POINT ( 'NONE',  ( -13.38449802415168932, -19.02034978033825396, 4.747874963382372471 ) ) ;
#5125 = CARTESIAN_POINT ( 'NONE',  ( 12.62155858231679417, -24.50000000000000000, 3.550687472877651629 ) ) ;
#5126 = CARTESIAN_POINT ( 'NONE',  ( -12.75496035233418013, -14.43700220713569138, 6.361037912489419632 ) ) ;
#5127 = CARTESIAN_POINT ( 'NONE',  ( -11.69094141768317741, -23.80360840875937001, 5.231925497173365081 ) ) ;
#5128 = ADVANCED_FACE ( 'NONE', ( #4715 ), #11104, .T. ) ;
#5129 = CARTESIAN_POINT ( 'NONE',  ( 15.00000000000000355, -30.00000000000000000, 1.000000000000000000 ) ) ;
#5130 = DIRECTION ( 'NONE',  ( 1.000000000000000000, 2.312964634635756072E-15, 0.000000000000000000 ) ) ;
#5131 = CARTESIAN_POINT ( 'NONE',  ( 11.96530858231679773, -20.97900456129165647, 3.863526089495444626 ) ) ;
#5132 = CARTESIAN_POINT ( 'NONE',  ( -5.784691417683177406, -23.77099543870834353, 4.174186261275251830 ) ) ;
#5133 = ORIENTED_EDGE ( 'NONE', *, *, #154, .T. ) ;
#5134 = ORIENTED_EDGE ( 'NONE', *, *, #18812, .F. ) ;
#5135 = ADVANCED_FACE ( 'NONE', ( #2095 ), #8479, .T. ) ;
#5136 = CARTESIAN_POINT ( 'NONE',  ( 13.38450946332969771, -19.76977210184853462, 5.359796180098093998 ) ) ;
#5137 = EDGE_CURVE ( 'NONE', #2654, #20035, #3867, .T. ) ;
#5138 = CARTESIAN_POINT ( 'NONE',  ( -18.98630159782011262, 9.000000000000001776, 1.000000000000000000 ) ) ;
#5139 = FACE_OUTER_BOUND ( 'NONE', #5080, .T. ) ;
#5140 = ORIENTED_EDGE ( 'NONE', *, *, #2501, .T. ) ;
#5141 = DIRECTION ( 'NONE',  ( 0.000000000000000000, 0.000000000000000000, 1.000000000000000000 ) ) ;
#5142 = DIRECTION ( 'NONE',  ( 0.000000000000000000, -0.000000000000000000, -1.000000000000000000 ) ) ;
#5143 = CARTESIAN_POINT ( 'NONE',  ( 13.77789853026076550, 0.09637577819625635367, 5.909013032956687006 ) ) ;
#5144 = CARTESIAN_POINT ( 'NONE',  ( 10.00000000000000355, -34.99999999999999289, 0.000000000000000000 ) ) ;
#5145 = CARTESIAN_POINT ( 'NONE',  ( 2.602174906157317835, -9.976397331638239052, 2.593889103792902606 ) ) ;
#5146 = LINE ( 'NONE', #11620, #7062 ) ;
#5147 = CARTESIAN_POINT ( 'NONE',  ( -12.64195242771744709, -19.39390240027112000, 5.496549442168085164 ) ) ;
#5148 = CARTESIAN_POINT ( 'NONE',  ( 5.777808582316794173, -20.27099543870833642, 2.724438792969431589 ) ) ;
#5149 = LINE ( 'NONE', #231, #18426 ) ;
#5150 = CARTESIAN_POINT ( 'NONE',  ( 13.12463908936614132, 4.981774012991869505, 5.264611377988129171 ) ) ;
#5151 = EDGE_CURVE ( 'NONE', #6462, #18369, #10444, .T. ) ;
#5152 = CARTESIAN_POINT ( 'NONE',  ( -1.957016269584227031, -9.152392576945766578, 2.382268221639079364 ) ) ;
#5153 = CARTESIAN_POINT ( 'NONE',  ( -13.87444723674697755, 4.972085455720938185, 5.163895512850782410 ) ) ;
#5154 = CARTESIAN_POINT ( 'NONE',  ( 0.000000000000000000, 10.00000000000000000, 1.000000000000000000 ) ) ;
#5155 = CARTESIAN_POINT ( 'NONE',  ( 11.97219141768317563, -23.72900456129165292, 2.724438792969417822 ) ) ;
#5156 = CARTESIAN_POINT ( 'NONE',  ( -8.215308582316795949, -23.02099543870833998, 3.136473910504556262 ) ) ;
#5157 = VERTEX_POINT ( 'NONE', #14846 ) ;
#5158 = CARTESIAN_POINT ( 'NONE',  ( 13.90326467458556969, 5.677366066573198644, 5.457668599364335904 ) ) ;
#5159 = CARTESIAN_POINT ( 'NONE',  ( 13.12529397354238192, 5.014845663890295846, 4.791666666666685614 ) ) ;
#5160 = CARTESIAN_POINT ( 'NONE',  ( 26.79469207716614676, 9.000000000000001776, 1.000000000000000000 ) ) ;
#5161 = ORIENTED_EDGE ( 'NONE', *, *, #8129, .T. ) ;
#5162 = VERTEX_POINT ( 'NONE', #14637 ) ;
#5163 = LINE ( 'NONE', #14679, #9119 ) ;
#5164 = FACE_OUTER_BOUND ( 'NONE', #16366, .T. ) ;
#5165 = DIRECTION ( 'NONE',  ( 1.000000000000000000, 0.000000000000000000, 0.000000000000000000 ) ) ;
#5166 = LINE ( 'NONE', #3703, #10335 ) ;
#5167 = CARTESIAN_POINT ( 'NONE',  ( 1.337453470010121714, -9.114917468222230923, 1.622643865078341463 ) ) ;
#5168 = CARTESIAN_POINT ( 'NONE',  ( -20.75349085826862350, 0.000000000000000000, 1.000000000000000000 ) ) ;
#5169 = FACE_OUTER_BOUND ( 'NONE', #18832, .T. ) ;
#5170 = EDGE_CURVE ( 'NONE', #18231, #14087, #1889, .T. ) ;
#5171 = CARTESIAN_POINT ( 'NONE',  ( 12.73094043006643616, -20.51123272440521816, 3.536703532973982433 ) ) ;
#5172 = DIRECTION ( 'NONE',  ( -1.000000000000000000, -1.013672804646636192E-16, 0.000000000000000000 ) ) ;
#5173 = CARTESIAN_POINT ( 'NONE',  ( -8.777808582316792396, -20.27099543870833642, 2.724438792969431589 ) ) ;
#5174 = EDGE_CURVE ( 'NONE', #20463, #2481, #16316, .T. ) ;
#5175 = CARTESIAN_POINT ( 'NONE',  ( -3.336296098497695262, -9.936854405034125648, 2.776348673047012383 ) ) ;
#5176 = ORIENTED_EDGE ( 'NONE', *, *, #174, .T. ) ;
#5177 = CARTESIAN_POINT ( 'NONE',  ( -12.62500004114794372, -19.49999792202770621, 4.520295319612473328 ) ) ;
#5178 = CARTESIAN_POINT ( 'NONE',  ( -12.05905858231679417, -20.72672167713054137, 4.701595411283463477 ) ) ;
#5179 = B_SPLINE_CURVE_WITH_KNOTS ( 'NONE', 3,
 ( #17883, #8569, #16310, #6592, #11807, #419 ),
 .UNSPECIFIED., .F., .F.,
 ( 4, 2, 4 ),
 ( 0.000000000000000000, 0.5000000000000000000, 1.000000000000000000 ),
 .UNSPECIFIED. ) ;
#5180 = CARTESIAN_POINT ( 'NONE',  ( -6.253441417683176518, -21.94931252712233061, 1.749999999999998446 ) ) ;
#5181 = ORIENTED_EDGE ( 'NONE', *, *, #11019, .T. ) ;
#5182 = CARTESIAN_POINT ( 'NONE',  ( 13.83531008031826026, 3.745659056069631898, 5.237458296715707284 ) ) ;
#5184 = DIRECTION ( 'NONE',  ( -1.000000000000000000, 0.000000000000000000, 0.000000000000000000 ) ) ;
#5183 = AXIS2_PLACEMENT_3D ( 'NONE', #10261, #7338, #18120 ) ;
#5185 = ORIENTED_EDGE ( 'NONE', *, *, #18702, .F. ) ;
#5186 = ORIENTED_EDGE ( 'NONE', *, *, #13582, .F. ) ;
#5187 = DIRECTION ( 'NONE',  ( 0.000000000000000000, 1.000000000000000000, 0.000000000000000000 ) ) ;
#5188 = ORIENTED_EDGE ( 'NONE', *, *, #356, .T. ) ;
#5189 = DIRECTION ( 'NONE',  ( 1.000000000000000000, 0.000000000000000000, 0.000000000000000000 ) ) ;
#5190 = VECTOR ( 'NONE', #15940, 1000.000000000000000 ) ;
#5191 = ORIENTED_EDGE ( 'NONE', *, *, #118, .F. ) ;
#5192 = CARTESIAN_POINT ( 'NONE',  ( 4.247260319564023945, 4.999999999999999112, 1.000000000000000000 ) ) ;
#5193 = CARTESIAN_POINT ( 'NONE',  ( 11.00000000000000000, -23.70993649053891517, 5.466506350946108483 ) ) ;
#5194 = PLANE ( 'NONE',  #11979 ) ;
#5195 = PLANE ( 'NONE',  #2988 ) ;
#5196 = DIRECTION ( 'NONE',  ( 0.000000000000000000, -0.000000000000000000, 1.000000000000000000 ) ) ;
#5197 = VECTOR ( 'NONE', #11017, 1000.000000000000000 ) ;
#5198 =( NAMED_UNIT ( * ) SI_UNIT ( $, .STERADIAN. ) SOLID_ANGLE_UNIT ( ) );
#5199 = EDGE_CURVE ( 'NONE', #3720, #9059, #14749, .T. ) ;
#5200 = CARTESIAN_POINT ( 'NONE',  ( 8.503441417683177406, -22.05068747287765873, 5.250000000000000888 ) ) ;
#5201 = CARTESIAN_POINT ( 'NONE',  ( -26.19203811574920593, 10.00000000000000000, 0.000000000000000000 ) ) ;
#5202 = CARTESIAN_POINT ( 'NONE',  ( -9.815941417683177406, -21.32873467460645145, 4.242948236979555254 ) ) ;
#5203 = ORIENTED_EDGE ( 'NONE', *, *, #5657, .T. ) ;
#5204 = CARTESIAN_POINT ( 'NONE',  ( 11.96530858231679773, -19.47900456129164937, 4.484846433055089676 ) ) ;
#5205 = CARTESIAN_POINT ( 'NONE',  ( 13.00900269284621302, -0.8578640112522492034, 5.903024842915844062 ) ) ;
#5206 = CARTESIAN_POINT ( 'NONE',  ( -13.15047398821051239, 5.536436404627260721, 5.896317606305554015 ) ) ;
#5207 = ORIENTED_EDGE ( 'NONE', *, *, #18074, .F. ) ;
#5208 = LINE ( 'NONE', #14829, #4272 ) ;
#5209 = DIRECTION ( 'NONE',  ( 0.000000000000000000, -0.000000000000000000, -1.000000000000000000 ) ) ;
#5210 = ORIENTED_EDGE ( 'NONE', *, *, #4777, .T. ) ;
#5211 = ORIENTED_EDGE ( 'NONE', *, *, #2333, .F. ) ;
#5212 = EDGE_CURVE ( 'NONE', #8633, #20067, #14945, .T. ) ;
#5213 = CARTESIAN_POINT ( 'NONE',  ( 13.36733061693429292, -20.15943224161095770, 3.450097756028646323 ) ) ;
#5214 = ORIENTED_EDGE ( 'NONE', *, *, #8761, .F. ) ;
#5215 = CARTESIAN_POINT ( 'NONE',  ( 9.000000000000000000, -9.999999999999991118, 2.000000000000000000 ) ) ;
#5216 = CARTESIAN_POINT ( 'NONE',  ( 13.02818618459764188, 0.1109023222084986743, 5.923858176248589125 ) ) ;
#5217 = CARTESIAN_POINT ( 'NONE',  ( -27.50000000000000711, 4.999999999999999112, 1.000000000000000000 ) ) ;
#5218 = CIRCLE ( 'NONE', #6894, 1.499999999999996225 ) ;
#5219 = CARTESIAN_POINT ( 'NONE',  ( 13.15498530132288479, 5.764257716805535559, 4.583333333333295734 ) ) ;
#5220 = CARTESIAN_POINT ( 'NONE',  ( 13.49999999999998401, -21.99999999999999645, 11.68378559369222280 ) ) ;
#5221 = CARTESIAN_POINT ( 'NONE',  ( -13.37561105820882013, -20.21914156045197686, 4.753815841436231260 ) ) ;
#5222 = CARTESIAN_POINT ( 'NONE',  ( 8.496558582316795949, -22.05068747287764452, 0.9999999999999978906 ) ) ;
#5223 = CARTESIAN_POINT ( 'NONE',  ( -13.13084019862132479, 4.544930030374419339, 6.677052771569639944 ) ) ;
#5224 = CARTESIAN_POINT ( 'NONE',  ( -6.809058582316796837, -23.80360840875935935, 1.768074502826626260 ) ) ;
#5225 = DIRECTION ( 'NONE',  ( -6.938893903907232322E-16, 1.000000000000000000, 0.000000000000000000 ) ) ;
#5226 = CARTESIAN_POINT ( 'NONE',  ( 3.944195004867014909, -21.56714562517547051, 5.389209506672564487 ) ) ;
#5227 = AXIS2_PLACEMENT_3D ( 'NONE', #4353, #5823, #1219 ) ;
#5228 = CARTESIAN_POINT ( 'NONE',  ( 8.684058582316795949, -21.32873467460644079, 2.757051763020455404 ) ) ;
#5229 = CARTESIAN_POINT ( 'NONE',  ( -5.503441417683176518, -22.05068747287765873, 5.250000000000000888 ) ) ;
#5230 = ORIENTED_EDGE ( 'NONE', *, *, #82, .F. ) ;
#5231 = EDGE_LOOP ( 'NONE', ( #2530, #15186, #6629, #10491, #4571 ) ) ;
#5232 = CARTESIAN_POINT ( 'NONE',  ( 13.87470602645761986, 4.985154336109792972, 3.666666666666500873 ) ) ;
#5233 = CARTESIAN_POINT ( 'NONE',  ( 20.49999999999998224, -21.99999999999999645, 12.00000000000000355 ) ) ;
#5234 =( LENGTH_UNIT ( ) NAMED_UNIT ( * ) SI_UNIT ( .MILLI., .METRE. ) );
#5235 = ORIENTED_EDGE ( 'NONE', *, *, #1486, .F. ) ;
#5236 = CARTESIAN_POINT ( 'NONE',  ( 13.92791111847407848, 4.999999999999999112, 1.000000000000000000 ) ) ;
#5237 = CARTESIAN_POINT ( 'NONE',  ( 11.00000000000000000, -19.49999999999999645, 4.000000000000000000 ) ) ;
#5238 = CARTESIAN_POINT ( 'NONE',  ( -24.79469207716615031, 0.000000000000000000, 1.000000000000000000 ) ) ;
#5239 = EDGE_CURVE ( 'NONE', #15313, #886, #16220, .T. ) ;
#5240 = CARTESIAN_POINT ( 'NONE',  ( 13.38800411018677572, -19.59329243556743805, 5.436267741224407146 ) ) ;
#5241 = LINE ( 'NONE', #17903, #508 ) ;
#5242 = CARTESIAN_POINT ( 'NONE',  ( 1.904508877737772998, -9.138371295333994837, 2.378667276417936627 ) ) ;
#5243 = CARTESIAN_POINT ( 'NONE',  ( 0.5631383031621635116, -9.114917468222230923, 1.622643865078341463 ) ) ;
#5244 = CARTESIAN_POINT ( 'NONE',  ( -12.72590726430969532, -14.40418315237199742, 4.861678440007700885 ) ) ;
#5245 = CARTESIAN_POINT ( 'NONE',  ( 7.465308582316795061, -20.22900456129164937, 4.174186261275266929 ) ) ;
#5246 = CARTESIAN_POINT ( 'NONE',  ( 0.000000000000000000, 0.000000000000000000, 4.000000000000000000 ) ) ;
#5247 = CARTESIAN_POINT ( 'NONE',  ( 12.79798428357658047, -11.51429367935891790, 5.673858176248284479 ) ) ;
#5248 = CARTESIAN_POINT ( 'NONE',  ( -1.655860418491166941, -9.114909740826840689, 2.372641880528837621 ) ) ;
#5249 = CARTESIAN_POINT ( 'NONE',  ( 8.496558582316795949, -22.05068747287764452, 2.499999999999999112 ) ) ;
#5250 = VECTOR ( 'NONE', #17358, 1000.000000000000000 ) ;
#5251 = CARTESIAN_POINT ( 'NONE',  ( 11.03469141768318273, -20.22900456129164581, 2.825813738724747726 ) ) ;
#5252 = CARTESIAN_POINT ( 'NONE',  ( -5.496558582316795949, -22.05068747287764452, 2.499999999999999112 ) ) ;
#5253 = ORIENTED_EDGE ( 'NONE', *, *, #20182, .F. ) ;
#5254 = CARTESIAN_POINT ( 'NONE',  ( 13.84517967659089521, 2.744073667841084418, 6.715984435864265301 ) ) ;
#5255 = CARTESIAN_POINT ( 'NONE',  ( 13.12529380813666435, 5.014837310896125722, 5.033295791462342628 ) ) ;
#5256 = VECTOR ( 'NONE', #17352, 1000.000000000000000 ) ;
#5257 = LINE ( 'NONE', #12895, #20713 ) ;
#5258 = ORIENTED_EDGE ( 'NONE', *, *, #14014, .F. ) ;
#5259 = VERTEX_POINT ( 'NONE', #10045 ) ;
#5260 = CARTESIAN_POINT ( 'NONE',  ( 32.65117217603048516, 6.460468870412194420, 0.000000000000000000 ) ) ;
#5261 = ADVANCED_FACE ( 'NONE', ( #12965 ), #522, .T. ) ;
#5262 = CARTESIAN_POINT ( 'NONE',  ( -13.50000000000000178, 5.000000000000047962, 4.000000000000000000 ) ) ;
#5263 = CARTESIAN_POINT ( 'NONE',  ( 15.00000000000000355, -5.999999999999996447, 2.000000000000000000 ) ) ;
#5264 = ADVANCED_FACE ( 'NONE', ( #6902 ), #3768, .T. ) ;
#5265 = CARTESIAN_POINT ( 'NONE',  ( -2.693754455098655409, -10.14181605509423711, 1.874202551270839123 ) ) ;
#5266 = CARTESIAN_POINT ( 'NONE',  ( 0.9854920305337622199, -9.864917468222230923, 1.622643865078341907 ) ) ;
#5267 = DIRECTION ( 'NONE',  ( 0.000000000000000000, 0.000000000000000000, -1.000000000000000000 ) ) ;
#5268 = EDGE_CURVE ( 'NONE', #18649, #15262, #19669, .T. ) ;
#5269 = LINE ( 'NONE', #14888, #9062 ) ;
#5270 = AXIS2_PLACEMENT_3D ( 'NONE', #4058, #7512, #18498 ) ;
#5271 = AXIS2_PLACEMENT_3D ( 'NONE', #2784, #8853, #5916 ) ;
#5272 = DIRECTION ( 'NONE',  ( 0.000000000000000000, 0.000000000000000000, 1.000000000000000000 ) ) ;
#5273 = CARTESIAN_POINT ( 'NONE',  ( 29.71062960567705602, 11.64110105645932691, 0.000000000000000000 ) ) ;
#5274 = CARTESIAN_POINT ( 'NONE',  ( -9.434058582316794173, -23.20159541128345992, 4.773278322869455970 ) ) ;
#5275 = CARTESIAN_POINT ( 'NONE',  ( -3.779650890485476200, -11.92851441922421607, 2.537846752097290715 ) ) ;
#5276 = EDGE_LOOP ( 'NONE', ( #20683, #14495, #20184, #17727 ) ) ;
#5277 = CARTESIAN_POINT ( 'NONE',  ( -12.93692567357942202, -3.747753484270499591, 5.090845106672844622 ) ) ;
#5278 = CARTESIAN_POINT ( 'NONE',  ( -9.715308582316794173, -23.77099543870833998, 2.825813738724734847 ) ) ;
#5279 = CARTESIAN_POINT ( 'NONE',  ( -9.722191417683177406, -20.27099543870833998, 4.275561207030583510 ) ) ;
#5280 = ORIENTED_EDGE ( 'NONE', *, *, #17117, .F. ) ;
#5281 = CARTESIAN_POINT ( 'NONE',  ( 13.47561960997282071, -14.41870969638424071, 4.846833296715798767 ) ) ;
#5282 =( NAMED_UNIT ( * ) PLANE_ANGLE_UNIT ( ) SI_UNIT ( $, .RADIAN. ) );
#5283 = ORIENTED_EDGE ( 'NONE', *, *, #8211, .T. ) ;
#5284 = ORIENTED_EDGE ( 'NONE', *, *, #12509, .F. ) ;
#5285 = DIRECTION ( 'NONE',  ( 0.4999999999999948930, 0.8660254037844415942, -0.000000000000000000 ) ) ;
#5286 = ORIENTED_EDGE ( 'NONE', *, *, #2791, .F. ) ;
#5287 = DIRECTION ( 'NONE',  ( 0.000000000000000000, -1.000000000000000000, 0.000000000000000000 ) ) ;
#5288 = EDGE_CURVE ( 'NONE', #7441, #5651, #5442, .T. ) ;
#5289 = VERTEX_POINT ( 'NONE', #6805 ) ;
#5290 = CARTESIAN_POINT ( 'NONE',  ( 6.628441417683176518, -20.24999999999999289, 3.550687472877664952 ) ) ;
#5291 = DIRECTION ( 'NONE',  ( 0.000000000000000000, 0.000000000000000000, 1.000000000000000000 ) ) ;
#5292 = DIRECTION ( 'NONE',  ( -0.000000000000000000, -0.000000000000000000, -1.000000000000000000 ) ) ;
#5293 = VECTOR ( 'NONE', #1085, 1000.000000000000000 ) ;
#5294 = CARTESIAN_POINT ( 'NONE',  ( -15.49999999999999822, -22.99999999999999289, 4.000000000000000000 ) ) ;
#5295 = CARTESIAN_POINT ( 'NONE',  ( -5.402808582316794173, -22.77556120703056308, 1.770995438708340197 ) ) ;
#5296 = VECTOR ( 'NONE', #7060, 1000.000000000000000 ) ;
#5297 = DIRECTION ( 'NONE',  ( -5.782411586589356653E-16, 1.000000000000000000, -0.000000000000000000 ) ) ;
#5298 = VECTOR ( 'NONE', #2701, 1000.000000000000000 ) ;
#5299 = CARTESIAN_POINT ( 'NONE',  ( 12.06594141768317563, -23.20159541128344927, 2.226721677130534705 ) ) ;
#5300 = DIRECTION ( 'NONE',  ( 0.000000000000000000, -1.000000000000000000, 0.000000000000000000 ) ) ;
#5301 = EDGE_CURVE ( 'NONE', #5810, #16102, #13174, .T. ) ;
#5302 = CARTESIAN_POINT ( 'NONE',  ( -5.597191417683177406, -22.46490103525075810, 4.479004561291653808 ) ) ;
#5303 = CARTESIAN_POINT ( 'NONE',  ( -9.434058582316795949, -23.73192549717337130, 5.303608408759367343 ) ) ;
#5304 = ORIENTED_EDGE ( 'NONE', *, *, #18166, .F. ) ;
#5305 = CARTESIAN_POINT ( 'NONE',  ( 12.74043380832193684, -14.42059267975384529, 5.611358176248560703 ) ) ;
#5306 = CARTESIAN_POINT ( 'NONE',  ( -12.62599079447150885, -20.19996487918709249, 4.820256282269618886 ) ) ;
#5307 = ORIENTED_EDGE ( 'NONE', *, *, #12271, .F. ) ;
#5308 = CARTESIAN_POINT ( 'NONE',  ( -7.500000000000000000, -23.70993649053891517, 5.466506350946108483 ) ) ;
#5309 = LINE ( 'NONE', #10021, #13006 ) ;
#5310 = ORIENTED_EDGE ( 'NONE', *, *, #17168, .F. ) ;
#5311 = VECTOR ( 'NONE', #12117, 1000.000000000000000 ) ;
#5312 = AXIS2_PLACEMENT_3D ( 'NONE', #12370, #1089, #12163 ) ;
#5313 = APPLICATION_PROTOCOL_DEFINITION ( 'draft international standard', 'automotive_design', 1998, #1200 ) ;
#5314 = ORIENTED_EDGE ( 'NONE', *, *, #1849, .F. ) ;
#5315 = ADVANCED_FACE ( 'NONE', ( #11509 ), #8377, .T. ) ;
#5316 = AXIS2_PLACEMENT_3D ( 'NONE', #15367, #17456, #18727 ) ;
#5317 = FACE_OUTER_BOUND ( 'NONE', #10934, .T. ) ;
#5318 = ADVANCED_FACE ( 'NONE', ( #19783 ), #3556, .F. ) ;
#5319 = VECTOR ( 'NONE', #586, 1000.000000000000000 ) ;
#5320 = ORIENTED_EDGE ( 'NONE', *, *, #15642, .F. ) ;
#5321 = CARTESIAN_POINT ( 'NONE',  ( -0.000000000000000000, 0.000000000000000000, 0.000000000000000000 ) ) ;
#5322 = CARTESIAN_POINT ( 'NONE',  ( 13.12526104302547836, 5.013182672784613381, 5.066812735559260261 ) ) ;
#5323 = LINE ( 'NONE', #16134, #5679 ) ;
#5324 = DIRECTION ( 'NONE',  ( 1.000000000000000000, 0.000000000000000000, 0.000000000000000000 ) ) ;
#5325 = CARTESIAN_POINT ( 'NONE',  ( 12.62499999999998579, -20.24999999999999289, 3.146526952850934755 ) ) ;
#5326 = CARTESIAN_POINT ( 'NONE',  ( 7.499999999999999112, -18.49999999999999645, 4.000000000000000000 ) ) ;
#5327 = VECTOR ( 'NONE', #18478, 1000.000000000000000 ) ;
#5328 = CARTESIAN_POINT ( 'NONE',  ( 7.465308582316796837, -19.47900456129164937, 4.484846433055089676 ) ) ;
#5329 = CARTESIAN_POINT ( 'NONE',  ( -13.15498530132288479, 5.764257716805535559, 4.833333333333343695 ) ) ;
#5330 = EDGE_CURVE ( 'NONE', #9626, #6206, #9937, .T. ) ;
#5331 = CARTESIAN_POINT ( 'NONE',  ( -7.277808582316795061, -19.52099543870833642, 2.413778621189609286 ) ) ;
#5332 = AXIS2_PLACEMENT_3D ( 'NONE', #18395, #10443, #2480 ) ;
#5333 = CARTESIAN_POINT ( 'NONE',  ( -23.35856191738413656, 9.000000000000001776, 0.000000000000000000 ) ) ;
#5334 = CARTESIAN_POINT ( 'NONE',  ( 0.000000000000000000, 16.00000000000000000, 1.000000000000000000 ) ) ;
#5335 = VECTOR ( 'NONE', #13372, 1000.000000000000000 ) ;
#5336 = CARTESIAN_POINT ( 'NONE',  ( 11.87155858231679595, -20.99999999999999645, 3.449312527122348371 ) ) ;
#5337 = FACE_OUTER_BOUND ( 'NONE', #8410, .T. ) ;
#5338 = ORIENTED_EDGE ( 'NONE', *, *, #6586, .F. ) ;
#5339 = ORIENTED_EDGE ( 'NONE', *, *, #7162, .T. ) ;
#5340 = CARTESIAN_POINT ( 'NONE',  ( 13.87470602645415063, 4.985154336109792972, 3.333333333332063830 ) ) ;
#5341 = FACE_OUTER_BOUND ( 'NONE', #3281, .T. ) ;
#5342 = CARTESIAN_POINT ( 'NONE',  ( -26.94203811574920593, 11.64110105645932691, 10.00000000000000000 ) ) ;
#5343 = ORIENTED_EDGE ( 'NONE', *, *, #19264, .F. ) ;
#5344 = CARTESIAN_POINT ( 'NONE',  ( -5.999999999999999112, -2.500000000000047518, 2.000000000000000000 ) ) ;
#5345 = FACE_OUTER_BOUND ( 'NONE', #18911, .T. ) ;
#5346 = CARTESIAN_POINT ( 'NONE',  ( 13.87470602645761808, 4.985154336109792972, 4.000000000000000000 ) ) ;
#5347 = CARTESIAN_POINT ( 'NONE',  ( 13.85343352903393388, 3.910893216212274925, 5.991044282956552891 ) ) ;
#5348 =( GEOMETRIC_REPRESENTATION_CONTEXT ( 3 ) GLOBAL_UNCERTAINTY_ASSIGNED_CONTEXT ( ( #3518 ) ) GLOBAL_UNIT_ASSIGNED_CONTEXT ( ( #13277, #13183, #9842 ) ) REPRESENTATION_CONTEXT ( 'NONE', 'WORKASPACE' ) );
#5349 = LINE ( 'NONE', #13700, #7857 ) ;
#5350 = CARTESIAN_POINT ( 'NONE',  ( 0.000000000000000000, -9.114917468222230923, 2.372643865078340575 ) ) ;
#5351 = VECTOR ( 'NONE', #9846, 1000.000000000000000 ) ;
#5352 = CARTESIAN_POINT ( 'NONE',  ( 1.819865260185086875, -9.122006307963404836, 1.624464420737683046 ) ) ;
#5353 = CARTESIAN_POINT ( 'NONE',  ( -13.04243487821393721, 1.580461349787872782, 5.205428440007538349 ) ) ;
#5354 = CARTESIAN_POINT ( 'NONE',  ( 7.277808582316795061, -20.27099543870833642, 2.724438792969431589 ) ) ;
#5355 = DIRECTION ( 'NONE',  ( 0.000000000000000000, 0.000000000000000000, 1.000000000000000000 ) ) ;
#5356 = CARTESIAN_POINT ( 'NONE',  ( 12.65051119073526564, -18.96168486786632457, 5.513701926248478102 ) ) ;
#5357 = EDGE_CURVE ( 'NONE', #9608, #11456, #19885, .T. ) ;
#5358 = CARTESIAN_POINT ( 'NONE',  ( -2.623717082130370137, -10.12934627674766830, 2.633169448359191644 ) ) ;
#5359 = CARTESIAN_POINT ( 'NONE',  ( 12.15280858231679950, -21.53509896474924901, 4.479004561291659137 ) ) ;
#5360 = CARTESIAN_POINT ( 'NONE',  ( 10.75344141768317741, -21.94931252712233061, 1.749999999999998446 ) ) ;
#5361 = CARTESIAN_POINT ( 'NONE',  ( -9.059058582316795949, -21.25705176302045274, 4.171265325393551215 ) ) ;
#5362 = ORIENTED_EDGE ( 'NONE', *, *, #3743, .F. ) ;
#5363 = CARTESIAN_POINT ( 'NONE',  ( 13.11465082267961968, 3.727366545318180791, 6.751662912489328150 ) ) ;
#5364 = CARTESIAN_POINT ( 'NONE',  ( 13.09206359972826661, 4.086711786274932479, 5.245812454509717782 ) ) ;
#5365 = FACE_OUTER_BOUND ( 'NONE', #8801, .T. ) ;
#5366 = VECTOR ( 'NONE', #5807, 1000.000000000000000 ) ;
#5367 = VERTEX_POINT ( 'NONE', #10462 ) ;
#5368 = VECTOR ( 'NONE', #9571, 1000.000000000000000 ) ;
#5369 = ORIENTED_EDGE ( 'NONE', *, *, #14037, .T. ) ;
#5370 = CARTESIAN_POINT ( 'NONE',  ( -14.99999999999998224, -17.49999999999999645, 1.000000000000000000 ) ) ;
#5371 = DIRECTION ( 'NONE',  ( -0.000000000000000000, -0.000000000000000000, -1.000000000000000000 ) ) ;
#5372 = CIRCLE ( 'NONE', #4728, 0.2500000000000002220 ) ;
#5373 = LINE ( 'NONE', #11643, #8317 ) ;
#5374 = DIRECTION ( 'NONE',  ( -1.000000000000000000, -0.000000000000000000, -0.000000000000000000 ) ) ;
#5375 = CARTESIAN_POINT ( 'NONE',  ( 2.367358971471363649, -9.400572650371021410, 2.446005822389718087 ) ) ;
#5376 = CARTESIAN_POINT ( 'NONE',  ( 6.063547257480584207, 11.64110105645932691, 10.00000000000000000 ) ) ;
#5377 = CARTESIAN_POINT ( 'NONE',  ( 13.00209451496117374, 0.000000000000000000, 1.000000000000000000 ) ) ;
#5378 = AXIS2_PLACEMENT_3D ( 'NONE', #11020, #6419, #17389 ) ;
#5379 = FACE_OUTER_BOUND ( 'NONE', #1336, .T. ) ;
#5380 = CARTESIAN_POINT ( 'NONE',  ( -9.689245429134309973, 11.64110105645932691, 10.00000000000000000 ) ) ;
#5381 = CARTESIAN_POINT ( 'NONE',  ( -9.996558582316794173, -22.05068747287764452, 1.749999999999998446 ) ) ;
#5382 = CIRCLE ( 'NONE', #8393, 1.499999999999996225 ) ;
#5383 = CARTESIAN_POINT ( 'NONE',  ( -3.722205087890566144, -11.52065056559861134, 2.433099166587254558 ) ) ;
#5384 = ORIENTED_EDGE ( 'NONE', *, *, #12459, .F. ) ;
#5385 = CARTESIAN_POINT ( 'NONE',  ( -13.74418849449709512, -0.8559810278826442964, 5.138499963383082125 ) ) ;
#5386 = CARTESIAN_POINT ( 'NONE',  ( -8.496558582316794173, -22.05068747287764452, 1.749999999999998446 ) ) ;
#5387 = EDGE_CURVE ( 'NONE', #19732, #14809, #15159, .T. ) ;
#5388 = CARTESIAN_POINT ( 'NONE',  ( -6.909691417683177406, -21.32581373872474373, 5.270995438708348857 ) ) ;
#5389 = ORIENTED_EDGE ( 'NONE', *, *, #2777, .F. ) ;
#5390 = CARTESIAN_POINT ( 'NONE',  ( 13.38800411018677572, -19.59329243556743805, 5.436267741224407146 ) ) ;
#5391 = CARTESIAN_POINT ( 'NONE',  ( -10.49999999999999822, -9.999999999999992895, 1.000000000000000000 ) ) ;
#5392 = ORIENTED_EDGE ( 'NONE', *, *, #7241, .T. ) ;
#5393 = ORIENTED_EDGE ( 'NONE', *, *, #2849, .F. ) ;
#5394 = CARTESIAN_POINT ( 'NONE',  ( -14.99999999999998579, -18.49999999999999645, 1.000000000000000000 ) ) ;
#5395 = VERTEX_POINT ( 'NONE', #15257 ) ;
#5396 = DIRECTION ( 'NONE',  ( -3.469446951953611033E-15, 1.000000000000000000, 0.000000000000000000 ) ) ;
#5397 = EDGE_CURVE ( 'NONE', #19275, #4418, #5541, .T. ) ;
#5398 = EDGE_CURVE ( 'NONE', #122, #7075, #4278, .T. ) ;
#5399 = VECTOR ( 'NONE', #12884, 1000.000000000000000 ) ;
#5400 = ORIENTED_EDGE ( 'NONE', *, *, #9108, .T. ) ;
#5401 = CARTESIAN_POINT ( 'NONE',  ( -5.000000000000000000, -12.50000000000000000, 1.000000000000000000 ) ) ;
#5402 = FACE_OUTER_BOUND ( 'NONE', #14924, .T. ) ;
#5403 = DIRECTION ( 'NONE',  ( 0.000000000000000000, 1.000000000000000000, -0.000000000000000000 ) ) ;
#5404 = CARTESIAN_POINT ( 'NONE',  ( 1.717920576997000737, -9.114924032904250240, 2.372645551019823884 ) ) ;
#5405 = CARTESIAN_POINT ( 'NONE',  ( -8.590308582316794173, -21.32581373872472952, 1.729004561291657138 ) ) ;
#5406 = CARTESIAN_POINT ( 'NONE',  ( 13.90439735423812273, 5.734566389025032684, 4.583333333333295734 ) ) ;
#5407 = DIRECTION ( 'NONE',  ( 0.000000000000000000, -1.000000000000000000, 0.000000000000000000 ) ) ;
#5408 = CARTESIAN_POINT ( 'NONE',  ( 11.31594141768317741, -21.32873467460645145, 4.242948236979555254 ) ) ;
#5409 = CARTESIAN_POINT ( 'NONE',  ( -12.62499999999998224, -20.24999999999998934, 4.166666666666636765 ) ) ;
#5410 = CARTESIAN_POINT ( 'NONE',  ( -8.503441417683177406, -22.05068747287766229, 4.499999999999999112 ) ) ;
#5411 = AXIS2_PLACEMENT_3D ( 'NONE', #2191, #7011, #15053 ) ;
#5412 = ADVANCED_FACE ( 'NONE', ( #11911 ), #13892, .F. ) ;
#5413 = CARTESIAN_POINT ( 'NONE',  ( -9.152808582316795949, -20.91377862118960351, 5.979004561291660913 ) ) ;
#5414 = ORIENTED_EDGE ( 'NONE', *, *, #19382, .T. ) ;
#5415 = CARTESIAN_POINT ( 'NONE',  ( 13.10012427866737639, 3.743776072700027324, 6.001983176248468332 ) ) ;
#5416 = CARTESIAN_POINT ( 'NONE',  ( -12.62888984277510218, -20.05356293986039873, 5.111704976569332537 ) ) ;
#5417 = ORIENTED_EDGE ( 'NONE', *, *, #5846, .F. ) ;
#5418 = FACE_OUTER_BOUND ( 'NONE', #14110, .T. ) ;
#5419 = DIRECTION ( 'NONE',  ( -0.000000000000000000, -0.000000000000000000, -1.000000000000000000 ) ) ;
#5420 = VERTEX_POINT ( 'NONE', #2716 ) ;
#5421 = CONTEXT_DEPENDENT_SHAPE_REPRESENTATION ( #13342, #12668 ) ;
#5422 = VECTOR ( 'NONE', #19579, 1000.000000000000000 ) ;
#5423 = ORIENTED_EDGE ( 'NONE', *, *, #27, .F. ) ;
#5424 = DIRECTION ( 'NONE',  ( 0.000000000000000000, 0.000000000000000000, 1.000000000000000000 ) ) ;
#5425 = ORIENTED_EDGE ( 'NONE', *, *, #16145, .T. ) ;
#5426 = ADVANCED_FACE ( 'NONE', ( #5856 ), #19982, .T. ) ;
#5427 = DIRECTION ( 'NONE',  ( 0.000000000000000000, 0.000000000000000000, -1.000000000000000000 ) ) ;
#5428 = CIRCLE ( 'NONE', #2084, 1.499999999999998668 ) ;
#5429 = CARTESIAN_POINT ( 'NONE',  ( 13.12270769621861355, 4.884238659038159902, 5.513847264053151065 ) ) ;
#5430 = CARTESIAN_POINT ( 'NONE',  ( -3.049989092406311109, -8.938202327316346896, 1.769874869409437279 ) ) ;
#5431 = LINE ( 'NONE', #19973, #7024 ) ;
#5432 = DIRECTION ( 'NONE',  ( 1.000000000000000000, 0.000000000000000000, 0.000000000000000000 ) ) ;
#5433 = CARTESIAN_POINT ( 'NONE',  ( 13.09532840572934376, 3.501584489333809724, 5.996774842915142401 ) ) ;
#5434 = DIRECTION ( 'NONE',  ( 0.000000000000000000, 0.000000000000000000, -1.000000000000000000 ) ) ;
#5435 = CARTESIAN_POINT ( 'NONE',  ( 10.74655858231679595, -21.94931252712234127, 6.000000000000001776 ) ) ;
#5436 = CARTESIAN_POINT ( 'NONE',  ( -13.15498530131898214, 5.764257716805535559, 3.333333333333075466 ) ) ;
#5437 = CARTESIAN_POINT ( 'NONE',  ( -5.034691417683177406, -19.47900456129164581, 2.515153566944927199 ) ) ;
#5438 = EDGE_CURVE ( 'NONE', #4739, #13902, #8991, .T. ) ;
#5439 = EDGE_LOOP ( 'NONE', ( #16761, #12416, #8916, #5568 ) ) ;
#5440 = EDGE_CURVE ( 'NONE', #3175, #3061, #10560, .T. ) ;
#5441 = CARTESIAN_POINT ( 'NONE',  ( -4.174178364069194536E-16, 3.500000000000001332, 1.000000000000000000 ) ) ;
#5442 = LINE ( 'NONE', #13381, #12752 ) ;
#5443 = VECTOR ( 'NONE', #769, 1000.000000000000000 ) ;
#5444 = CARTESIAN_POINT ( 'NONE',  ( 7.559058582316795949, -21.25705176302045274, 4.171265325393551215 ) ) ;
#5445 = DIRECTION ( 'NONE',  ( 1.000000000000000000, 0.000000000000000000, 0.000000000000000000 ) ) ;
#5446 = ORIENTED_EDGE ( 'NONE', *, *, #19002, .T. ) ;
#5447 = ORIENTED_EDGE ( 'NONE', *, *, #1825, .T. ) ;
#5448 = CARTESIAN_POINT ( 'NONE',  ( 13.43259567872942917, -17.34141822415733714, 5.534013032956523581 ) ) ;
#5449 = DIRECTION ( 'NONE',  ( -0.000000000000000000, -0.000000000000000000, -1.000000000000000000 ) ) ;
#5450 = ORIENTED_EDGE ( 'NONE', *, *, #7749, .F. ) ;
#5451 = CARTESIAN_POINT ( 'NONE',  ( -3.997260319564023501, 9.000000000000001776, 1.000000000000000000 ) ) ;
#5452 = PLANE ( 'NONE',  #3030 ) ;
#5453 = EDGE_CURVE ( 'NONE', #13535, #3666, #16727, .T. ) ;
#5454 = DIRECTION ( 'NONE',  ( -5.204170427930446527E-15, 1.000000000000000000, 0.000000000000000000 ) ) ;
#5455 = CARTESIAN_POINT ( 'NONE',  ( 13.70116456325478893, -3.778689555664588973, 5.825679699621801433 ) ) ;
#5456 = CARTESIAN_POINT ( 'NONE',  ( -17.55017143803810242, 4.999999999999999112, 1.000000000000000000 ) ) ;
#5457 = CARTESIAN_POINT ( 'NONE',  ( 3.257364212367626966, -9.501732542047829355, 2.664600686199549706 ) ) ;
#5458 = CIRCLE ( 'NONE', #6469, 0.2500000000000002220 ) ;
#5459 = CARTESIAN_POINT ( 'NONE',  ( 1.720709671993384093, -9.114925383610804843, 1.622645897908254753 ) ) ;
#5460 = CARTESIAN_POINT ( 'NONE',  ( -12.63118877378512828, -19.18746692385052555, 4.758813856674282583 ) ) ;
#5461 = FILL_AREA_STYLE ('',( #12989 ) ) ;
#5462 = CARTESIAN_POINT ( 'NONE',  ( 0.000000000000000000, 4.999999999999999112, 1.000000000000000000 ) ) ;
#5463 = CARTESIAN_POINT ( 'NONE',  ( 12.74043380832193684, -14.42059267975384529, 5.611358176248560703 ) ) ;
#5464 = CARTESIAN_POINT ( 'NONE',  ( -1.824488249492779879, -9.124319963227819130, 2.375058613629473570 ) ) ;
#5465 = CARTESIAN_POINT ( 'NONE',  ( 9.996558582316795949, -22.05068747287764452, 2.499999999999999112 ) ) ;
#5466 = CARTESIAN_POINT ( 'NONE',  ( 9.159691417683179182, -22.67418626127524917, 1.729004561291651809 ) ) ;
#5467 = CARTESIAN_POINT ( 'NONE',  ( -9.996558582316794173, -22.05068747287764452, 1.749999999999998446 ) ) ;
#5468 = ORIENTED_EDGE ( 'NONE', *, *, #8876, .T. ) ;
#5469 = CARTESIAN_POINT ( 'NONE',  ( 13.14782865898149034, 5.402847278557675104, 6.092770214907355708 ) ) ;
#5470 = CARTESIAN_POINT ( 'NONE',  ( 12.70672377255832686, -15.37294948583620346, 4.840845106674187548 ) ) ;
#5471 = PLANE ( 'NONE',  #1989 ) ;
#5472 = ORIENTED_EDGE ( 'NONE', *, *, #9240, .F. ) ;
#5473 = ORIENTED_EDGE ( 'NONE', *, *, #17937, .F. ) ;
#5474 = LINE ( 'NONE', #16649, #7106 ) ;
#5475 = ADVANCED_FACE ( 'NONE', ( #18301 ), #9096, .T. ) ;
#5476 = LINE ( 'NONE', #16354, #17254 ) ;
#5477 = DIRECTION ( 'NONE',  ( 1.000000000000000000, -0.000000000000000000, 0.000000000000000000 ) ) ;
#5478 = FACE_OUTER_BOUND ( 'NONE', #5033, .T. ) ;
#5479 = CARTESIAN_POINT ( 'NONE',  ( 2.203959450683124377, -9.262433282444222371, 2.410528873095051594 ) ) ;
#5480 = DIRECTION ( 'NONE',  ( 0.000000000000000000, 0.000000000000000000, -1.000000000000000000 ) ) ;
#5481 = CARTESIAN_POINT ( 'NONE',  ( -24.87918902992234393, 10.00000000000000000, 1.000000000000000000 ) ) ;
#5482 = CARTESIAN_POINT ( 'NONE',  ( 13.06507523707239038, -20.62500821465549095, 3.491123088105135608 ) ) ;
#5483 = LINE ( 'NONE', #16560, #6654 ) ;
#5484 = CARTESIAN_POINT ( 'NONE',  ( -10.09030858231679595, -21.32581373872472597, 1.729004561291657582 ) ) ;
#5485 = CARTESIAN_POINT ( 'NONE',  ( 0.000000000000000000, -9.114917468222230923, 2.372643865078340575 ) ) ;
#5486 = ORIENTED_EDGE ( 'NONE', *, *, #2703, .F. ) ;
#5487 = CARTESIAN_POINT ( 'NONE',  ( -13.37499999999998224, -19.50000000000006040, 4.416666666666682062 ) ) ;
#5488 = CARTESIAN_POINT ( 'NONE',  ( -8.215308582316792396, -23.77099543870833998, 2.825813738724734847 ) ) ;
#5489 = CARTESIAN_POINT ( 'NONE',  ( -10.47219141768317741, -22.97900456129165292, 3.035098964749240125 ) ) ;
#5490 = VERTEX_POINT ( 'NONE', #17141 ) ;
#5491 = CARTESIAN_POINT ( 'NONE',  ( 13.58606361274418184, -9.591287556442823714, 5.700679699621803209 ) ) ;
#5492 = LINE ( 'NONE', #16784, #4707 ) ;
#5493 = ORIENTED_EDGE ( 'NONE', *, *, #4936, .F. ) ;
#5494 = VERTEX_POINT ( 'NONE', #16930 ) ;
#5495 = DIRECTION ( 'NONE',  ( 0.000000000000000000, 1.000000000000000000, -0.000000000000000000 ) ) ;
#5496 = ORIENTED_EDGE ( 'NONE', *, *, #16286, .T. ) ;
#5497 = CARTESIAN_POINT ( 'NONE',  ( -13.38450946332969771, -19.76977210184853462, 5.359796180098093998 ) ) ;
#5498 = ORIENTED_EDGE ( 'NONE', *, *, #4875, .T. ) ;
#5499 = CARTESIAN_POINT ( 'NONE',  ( 8.126396343307449754, 0.000000000000000000, 1.000000000000000000 ) ) ;
#5500 = DIRECTION ( 'NONE',  ( 0.1351665943404306014, -0.9596796555888912339, 0.2464649070825229438 ) ) ;
#5501 = EDGE_CURVE ( 'NONE', #3437, #20223, #9193, .T. ) ;
#5502 = FACE_OUTER_BOUND ( 'NONE', #9143, .T. ) ;
#5503 = CARTESIAN_POINT ( 'NONE',  ( 3.257364212367626966, -9.501732542047829355, 2.664600686199549706 ) ) ;
#5504 = CARTESIAN_POINT ( 'NONE',  ( -6.715308582316794173, -23.77099543870833998, 2.825813738724734847 ) ) ;
#5505 = CARTESIAN_POINT ( 'NONE',  ( 13.90439735423812273, 5.734566389025032684, 4.916666666666649199 ) ) ;
#5506 = CARTESIAN_POINT ( 'NONE',  ( -2.187849085826861550, 11.64110105645932691, 10.00000000000000000 ) ) ;
#5507 = EDGE_CURVE ( 'NONE', #7382, #12312, #15568, .T. ) ;
#5508 = VECTOR ( 'NONE', #9210, 1000.000000000000000 ) ;
#5509 = EDGE_CURVE ( 'NONE', #18680, #8532, #7218, .T. ) ;
#5510 = CARTESIAN_POINT ( 'NONE',  ( 9.347191417683177406, -21.53509896474923835, 2.520995438708346192 ) ) ;
#5511 = CARTESIAN_POINT ( 'NONE',  ( -12.62499999999998401, -20.24999999999998934, 2.439580858552613751 ) ) ;
#5512 = CARTESIAN_POINT ( 'NONE',  ( -8.784691417683177406, -23.02099543870834353, 3.863526089495429972 ) ) ;
#5513 = CARTESIAN_POINT ( 'NONE',  ( -10.46530858231679595, -19.47900456129164937, 4.484846433055089676 ) ) ;
#5514 = ORIENTED_EDGE ( 'NONE', *, *, #6104, .F. ) ;
#5515 = CARTESIAN_POINT ( 'NONE',  ( 13.12119116326504908, 4.807653744879115010, 5.626470997801169105 ) ) ;
#5516 = CARTESIAN_POINT ( 'NONE',  ( -12.66849571425264287, -18.05346643024382303, 5.533233176248494978 ) ) ;
#5517 = ORIENTED_EDGE ( 'NONE', *, *, #5913, .F. ) ;
#5518 = VECTOR ( 'NONE', #1321, 1000.000000000000000 ) ;
#5519 = CARTESIAN_POINT ( 'NONE',  ( 5.999999999999999112, -7.500000000000047073, 2.000000000000000000 ) ) ;
#5520 = CARTESIAN_POINT ( 'NONE',  ( -7.869520639128047002, 9.000000000000001776, 1.000000000000000000 ) ) ;
#5521 = CIRCLE ( 'NONE', #10495, 2.500000000000000444 ) ;
#5522 = ORIENTED_EDGE ( 'NONE', *, *, #7932, .F. ) ;
#5523 = EDGE_LOOP ( 'NONE', ( #20073, #2123, #15205, #11767 ) ) ;
#5524 = AXIS2_PLACEMENT_3D ( 'NONE', #4582, #6366, #1351 ) ;
#5525 = ORIENTED_EDGE ( 'NONE', *, *, #15152, .T. ) ;
#5526 = DIRECTION ( 'NONE',  ( -0.000000000000000000, -0.000000000000000000, -1.000000000000000000 ) ) ;
#5527 = CARTESIAN_POINT ( 'NONE',  ( 12.65410809543883985, -18.78004118034163739, 5.517608176248461227 ) ) ;
#5528 = ADVANCED_FACE ( 'NONE', ( #20196 ), #13484, .F. ) ;
#5529 = CARTESIAN_POINT ( 'NONE',  ( -1.337453470010121714, -8.364917468222230923, 1.622643865078341907 ) ) ;
#5530 = LINE ( 'NONE', #20080, #15376 ) ;
#5531 = FACE_OUTER_BOUND ( 'NONE', #16567, .T. ) ;
#5532 = CARTESIAN_POINT ( 'NONE',  ( 13.12529397354238192, 5.014845663890295846, 4.916666666666650087 ) ) ;
#5533 = LINE ( 'NONE', #4381, #14343 ) ;
#5534 = EDGE_CURVE ( 'NONE', #13135, #13151, #10353, .T. ) ;
#5535 = EDGE_CURVE ( 'NONE', #4699, #4291, #15363, .T. ) ;
#5536 = CARTESIAN_POINT ( 'NONE',  ( 5.590308582316795949, -21.01515356694490322, 0.9790045612916562501 ) ) ;
#5537 = CARTESIAN_POINT ( 'NONE',  ( -12.95145221759166354, -3.764163011652346569, 5.840524842913703552 ) ) ;
#5538 = CARTESIAN_POINT ( 'NONE',  ( -4.097191417683177406, -23.08622137881040359, 5.979004561291654696 ) ) ;
#5539 = ORIENTED_EDGE ( 'NONE', *, *, #1802, .T. ) ;
#5540 = DIRECTION ( 'NONE',  ( -1.000000000000000000, 0.000000000000000000, 0.000000000000000000 ) ) ;
#5541 = LINE ( 'NONE', #934, #10420 ) ;
#5542 = CARTESIAN_POINT ( 'NONE',  ( -13.83079205777725917, 2.017498917744843023, 6.700359435863729729 ) ) ;
#5543 = CARTESIAN_POINT ( 'NONE',  ( 6.434058582316796837, -22.67126532539354855, 4.242948236979545484 ) ) ;
#5544 = DIRECTION ( 'NONE',  ( 0.000000000000000000, 0.000000000000000000, -1.000000000000000000 ) ) ;
#5545 = VERTEX_POINT ( 'NONE', #5755 ) ;
#5546 = EDGE_LOOP ( 'NONE', ( #14357, #19986, #7203, #16280, #17408, #20074, #4949, #18567, #2695, #14752, #16809, #1697 ) ) ;
#5547 = CARTESIAN_POINT ( 'NONE',  ( 13.80667376788930056, 1.549525278393783179, 5.940263032956496048 ) ) ;
#5548 = DIRECTION ( 'NONE',  ( 0.000000000000000000, 0.8660254037844363761, -0.5000000000000041078 ) ) ;
#5549 = SURFACE_SIDE_STYLE ('',( #13493 ) ) ;
#5550 = VERTEX_POINT ( 'NONE', #18414 ) ;
#5551 = CARTESIAN_POINT ( 'NONE',  ( -2.499999999999998224, -24.49999999999999289, 1.000000000000000000 ) ) ;
#5552 = DIRECTION ( 'NONE',  ( 0.000000000000000000, -1.000000000000000000, 0.000000000000000000 ) ) ;
#5553 = PLANE ( 'NONE',  #11971 ) ;
#5554 = CARTESIAN_POINT ( 'NONE',  ( 13.37499999999998757, -20.24999999999999289, 3.482947684955674639 ) ) ;
#5555 = EDGE_CURVE ( 'NONE', #20689, #14130, #16831, .T. ) ;
#5556 = CARTESIAN_POINT ( 'NONE',  ( -23.35856191738413656, 0.000000000000000000, 1.000000000000000000 ) ) ;
#5557 = CARTESIAN_POINT ( 'NONE',  ( 3.343476823822036259, -9.987837386737346890, 2.789442121235767402 ) ) ;
#5558 = DIRECTION ( 'NONE',  ( -0.000000000000000000, -0.000000000000000000, -1.000000000000000000 ) ) ;
#5559 = CARTESIAN_POINT ( 'NONE',  ( -12.62515856830665584, -19.49199230051052822, 4.565864671500353467 ) ) ;
#5560 = DIRECTION ( 'NONE',  ( 0.000000000000000000, -0.000000000000000000, 1.000000000000000000 ) ) ;
#5561 = CARTESIAN_POINT ( 'NONE',  ( 11.96530858231679595, -20.22900456129164937, 4.174186261275266929 ) ) ;
#5562 = CARTESIAN_POINT ( 'NONE',  ( -13.45671396861735403, -16.87344458480707843, 6.294109435864141844 ) ) ;
#5563 = CARTESIAN_POINT ( 'NONE',  ( 3.747260319564023501, 9.000000000000001776, 1.000000000000000000 ) ) ;
#5564 = CARTESIAN_POINT ( 'NONE',  ( 12.71530858231679417, -23.02099543870833998, 3.136473910504556262 ) ) ;
#5565 = EDGE_CURVE ( 'NONE', #5007, #485, #1251, .T. ) ;
#5566 = CARTESIAN_POINT ( 'NONE',  ( 6.347191417683176518, -21.22443879296941915, 1.770995438708345748 ) ) ;
#5567 = CARTESIAN_POINT ( 'NONE',  ( -10.74655858231679417, -21.94931252712234482, 5.250000000000000888 ) ) ;
#5568 = ORIENTED_EDGE ( 'NONE', *, *, #7869, .F. ) ;
#5569 = CARTESIAN_POINT ( 'NONE',  ( 13.12405442816082868, 4.202248622120948518, 6.747400073346936367 ) ) ;
#5570 = CARTESIAN_POINT ( 'NONE',  ( 13.05202662408965075, 2.064844516520778939, 5.215845106673912213 ) ) ;
#5571 = DIRECTION ( 'NONE',  ( 1.000000000000000000, -0.000000000000000000, 0.000000000000000000 ) ) ;
#5572 = ORIENTED_EDGE ( 'NONE', *, *, #14394, .F. ) ;
#5573 = VERTEX_POINT ( 'NONE', #10974 ) ;
#5574 = LINE ( 'NONE', #8417, #9773 ) ;
#5575 = VECTOR ( 'NONE', #6250, 1000.000000000000000 ) ;
#5576 = CARTESIAN_POINT ( 'NONE',  ( 0.000000000000000000, 9.000000000000001776, 0.000000000000000000 ) ) ;
#5577 = EDGE_CURVE ( 'NONE', #12312, #2482, #13993, .T. ) ;
#5578 = ADVANCED_FACE ( 'NONE', ( #10876 ), #14409, .F. ) ;
#5579 = CARTESIAN_POINT ( 'NONE',  ( 21.25349085826861995, 16.00000000000000000, 1.000000000000000000 ) ) ;
#5580 = DIRECTION ( 'NONE',  ( 0.000000000000000000, 1.000000000000000000, -0.000000000000000000 ) ) ;
#5581 = CARTESIAN_POINT ( 'NONE',  ( 1.337453470010121714, -9.114917468222230923, 2.372643865078341019 ) ) ;
#5582 = FACE_OUTER_BOUND ( 'NONE', #15165, .T. ) ;
#5583 = AXIS2_PLACEMENT_3D ( 'NONE', #12031, #10889, #12139 ) ;
#5584 = LINE ( 'NONE', #19927, #13718 ) ;
#5585 = CARTESIAN_POINT ( 'NONE',  ( 12.66022036808238305, -20.41063448930580648, 3.546131378954796798 ) ) ;
#5586 = CARTESIAN_POINT ( 'NONE',  ( 0.000000000000000000, 4.999999999999999112, 1.000000000000000000 ) ) ;
#5587 = CARTESIAN_POINT ( 'NONE',  ( -5.215308582316793284, -23.77099543870833998, 2.825813738724734847 ) ) ;
#5588 = CARTESIAN_POINT ( 'NONE',  ( -3.385922596301560894, -9.481287983549590237, 1.909350115156127403 ) ) ;
#5589 = ORIENTED_EDGE ( 'NONE', *, *, #11713, .T. ) ;
#5590 = CARTESIAN_POINT ( 'NONE',  ( -13.37499994994395891, -19.50000252782794519, 4.474109982178703149 ) ) ;
#5591 = CARTESIAN_POINT ( 'NONE',  ( -4.687312169500632564, -21.51559725698341197, 5.182386163300427562 ) ) ;
#5592 = EDGE_CURVE ( 'NONE', #15085, #13339, #3396, .T. ) ;
#5593 = CARTESIAN_POINT ( 'NONE',  ( 9.996558582316795949, -22.05068747287764452, 0.9999999999999978906 ) ) ;
#5594 = CARTESIAN_POINT ( 'NONE',  ( -12.34719141768317741, -21.53509896474923835, 2.520995438708346192 ) ) ;
#5595 = ORIENTED_EDGE ( 'NONE', *, *, #7459, .T. ) ;
#5596 = CARTESIAN_POINT ( 'NONE',  ( 13.85223456079946303, 3.850345320370711644, 5.989742199623227847 ) ) ;
#5597 = LINE ( 'NONE', #20043, #3046 ) ;
#5598 = ORIENTED_EDGE ( 'NONE', *, *, #14003, .T. ) ;
#5599 = ORIENTED_EDGE ( 'NONE', *, *, #2749, .F. ) ;
#5600 = DIRECTION ( 'NONE',  ( 0.000000000000000000, -0.000000000000000000, 1.000000000000000000 ) ) ;
#5601 = ORIENTED_EDGE ( 'NONE', *, *, #6527, .F. ) ;
#5602 = CARTESIAN_POINT ( 'NONE',  ( -13.37524505148396514, -20.23762490005974968, 4.659512268729234741 ) ) ;
#5603 = ORIENTED_EDGE ( 'NONE', *, *, #1709, .T. ) ;
#5604 = CARTESIAN_POINT ( 'NONE',  ( -12.50209451496117197, 16.00000000000000000, 1.000000000000000000 ) ) ;
#5605 = AXIS2_PLACEMENT_3D ( 'NONE', #7527, #5540, #13483 ) ;
#5606 = DIRECTION ( 'NONE',  ( 0.000000000000000000, -1.000000000000000000, 0.000000000000000000 ) ) ;
#5607 = DIRECTION ( 'NONE',  ( -1.000000000000000000, 0.000000000000000000, 0.000000000000000000 ) ) ;
#5608 = CARTESIAN_POINT ( 'NONE',  ( 3.767139617958116471, -12.99583330722436791, 3.561955564372631500 ) ) ;
#5609 = CARTESIAN_POINT ( 'NONE',  ( -5.309058582316794173, -23.27327832286945153, 2.298404588716537411 ) ) ;
#5610 = CARTESIAN_POINT ( 'NONE',  ( 12.62499999999998224, -21.00000000000006395, 4.416666666666682062 ) ) ;
#5611 = DIRECTION ( 'NONE',  ( 0.000000000000000000, 0.000000000000000000, 1.000000000000000000 ) ) ;
#5612 = CARTESIAN_POINT ( 'NONE',  ( 11.78469141768317741, -23.02099543870834353, 3.863526089495429972 ) ) ;
#5613 = CARTESIAN_POINT ( 'NONE',  ( -12.62499999999998579, -20.24999999999999289, 3.146526952850934755 ) ) ;
#5614 = CARTESIAN_POINT ( 'NONE',  ( -5.128441417683177406, -20.99999999999999645, 3.550687472877664952 ) ) ;
#5615 = EDGE_CURVE ( 'NONE', #20251, #17893, #3227, .T. ) ;
#5616 = CARTESIAN_POINT ( 'NONE',  ( -12.62844141768317741, -19.49999999999998934, 3.550687472877664952 ) ) ;
#5617 = PRESENTATION_LAYER_ASSIGNMENT (  '', '', ( #7955 ) ) ;
#5618 = ORIENTED_EDGE ( 'NONE', *, *, #19739, .T. ) ;
#5619 = CARTESIAN_POINT ( 'NONE',  ( 12.67794853492974561, -16.82609898603114118, 4.809595106674325216 ) ) ;
#5620 = CARTESIAN_POINT ( 'NONE',  ( -12.65650603190776025, -18.65894538865861563, 5.520212342915047365 ) ) ;
#5621 = ORIENTED_EDGE ( 'NONE', *, *, #15464, .T. ) ;
#5622 = AXIS2_PLACEMENT_3D ( 'NONE', #10127, #6787, #13054 ) ;
#5623 = EDGE_CURVE ( 'NONE', #8041, #3395, #20510, .T. ) ;
#5624 = CARTESIAN_POINT ( 'NONE',  ( -20.00349085826861995, 16.00000000000000000, 1.000000000000000000 ) ) ;
#5625 = CARTESIAN_POINT ( 'NONE',  ( 12.25209451496117197, 10.00000000000000000, 1.000000000000000000 ) ) ;
#5626 = ORIENTED_EDGE ( 'NONE', *, *, #10789, .T. ) ;
#5627 = EDGE_LOOP ( 'NONE', ( #4985, #8971, #15114, #498 ) ) ;
#5628 = EDGE_LOOP ( 'NONE', ( #8691, #710, #13444, #13775 ) ) ;
#5629 = LINE ( 'NONE', #12005, #16653 ) ;
#5630 = LINE ( 'NONE', #4065, #3592 ) ;
#5631 = VECTOR ( 'NONE', #12030, 1000.000000000000000 ) ;
#5632 = CARTESIAN_POINT ( 'NONE',  ( -3.451003380014874722, -9.682417022083358304, 1.961004070207825523 ) ) ;
#5633 = DIRECTION ( 'NONE',  ( -0.000000000000000000, -0.000000000000000000, -1.000000000000000000 ) ) ;
#5634 = FACE_BOUND ( 'NONE', #13608, .T. ) ;
#5635 = VECTOR ( 'NONE', #13885, 1000.000000000000000 ) ;
#5636 = VECTOR ( 'NONE', #17223, 1000.000000000000000 ) ;
#5637 = FACE_OUTER_BOUND ( 'NONE', #13589, .T. ) ;
#5638 = CARTESIAN_POINT ( 'NONE',  ( 6.715308582316796837, -24.52099543870834708, 2.515153566944913432 ) ) ;
#5639 = CARTESIAN_POINT ( 'NONE',  ( -13.11740841389447709, 4.616624901677048420, 5.813473370769506765 ) ) ;
#5640 = CARTESIAN_POINT ( 'NONE',  ( -6.347191417683176518, -20.91377862118959285, 1.020995438708345082 ) ) ;
#5641 = ORIENTED_EDGE ( 'NONE', *, *, #18837, .T. ) ;
#5642 = CARTESIAN_POINT ( 'NONE',  ( 11.59030858231679417, -21.32581373872472597, 1.729004561291657582 ) ) ;
#5643 = DIRECTION ( 'NONE',  ( 0.000000000000000000, 0.000000000000000000, -1.000000000000000000 ) ) ;
#5644 = CARTESIAN_POINT ( 'NONE',  ( -13.44712222274167246, -17.35782775154002522, 6.283692769197384287 ) ) ;
#5645 = VECTOR ( 'NONE', #16685, 1000.000000000000000 ) ;
#5646 = EDGE_CURVE ( 'NONE', #14589, #11516, #9598, .T. ) ;
#5647 = CARTESIAN_POINT ( 'NONE',  ( 11.77780858231679417, -20.27099543870833642, 2.724438792969431589 ) ) ;
#5648 = CARTESIAN_POINT ( 'NONE',  ( 0.000000000000000000, 9.000000000000001776, 0.000000000000000000 ) ) ;
#5649 = AXIS2_PLACEMENT_3D ( 'NONE', #16298, #3231, #5209 ) ;
#5650 = ORIENTED_EDGE ( 'NONE', *, *, #19626, .F. ) ;
#5651 = VERTEX_POINT ( 'NONE', #12433 ) ;
#5652 = CARTESIAN_POINT ( 'NONE',  ( 13.75871503850933841, -0.8723905552644914962, 5.888179699623941943 ) ) ;
#5653 = DIRECTION ( 'NONE',  ( 1.000000000000000000, 0.000000000000000000, 0.000000000000000000 ) ) ;
#5654 = SURFACE_STYLE_FILL_AREA ( #844 ) ;
#5655 = EDGE_LOOP ( 'NONE', ( #8768, #3467, #13427, #14466 ) ) ;
#5656 = CARTESIAN_POINT ( 'NONE',  ( -7.369520639128046113, 0.000000000000000000, 0.000000000000000000 ) ) ;
#5657 = EDGE_CURVE ( 'NONE', #8747, #11334, #17551, .T. ) ;
#5658 = EDGE_CURVE ( 'NONE', #6686, #18235, #2919, .T. ) ;
#5659 = CARTESIAN_POINT ( 'NONE',  ( -5.433390479346035029, 4.999999999999999112, 1.000000000000000000 ) ) ;
#5660 = DIRECTION ( 'NONE',  ( 1.000000000000000000, 0.000000000000000000, 0.000000000000000000 ) ) ;
#5661 = CARTESIAN_POINT ( 'NONE',  ( -13.00000000000000355, 0.000000000000000000, 1.000000000000000000 ) ) ;
#5662 = CIRCLE ( 'NONE', #17346, 2.999999999999999112 ) ;
#5663 = CARTESIAN_POINT ( 'NONE',  ( -13.49999999999998401, -18.49999999999999645, 4.000000000000000000 ) ) ;
#5664 = CARTESIAN_POINT ( 'NONE',  ( 1.407845757905374695, -9.114917468222230923, 2.372643865078341019 ) ) ;
#5665 = AXIS2_PLACEMENT_3D ( 'NONE', #7460, #7152, #4107 ) ;
#5666 = CARTESIAN_POINT ( 'NONE',  ( 5.000000000000000000, -12.50000000000000000, 4.500000000000000888 ) ) ;
#5667 = CARTESIAN_POINT ( 'NONE',  ( -12.63958155142659834, -18.76363165295958524, 4.767928440007602298 ) ) ;
#5668 = DIRECTION ( 'NONE',  ( 0.000000000000000000, -1.000000000000000000, 0.000000000000000000 ) ) ;
#5669 = CARTESIAN_POINT ( 'NONE',  ( 11.02780858231679595, -23.72900456129165647, 4.275561207030568411 ) ) ;
#5670 = CARTESIAN_POINT ( 'NONE',  ( -13.39995901559228031, -19.73956971259024229, 6.178279423016713956 ) ) ;
#5671 = CARTESIAN_POINT ( 'NONE',  ( 23.10856191738414012, 4.999999999999999112, 1.000000000000000000 ) ) ;
#5672 = CARTESIAN_POINT ( 'NONE',  ( 13.37155858231679417, -20.24999999999999289, 3.449312527122348371 ) ) ;
#5673 = EDGE_CURVE ( 'NONE', #18307, #18399, #17451, .T. ) ;
#5674 = CARTESIAN_POINT ( 'NONE',  ( 12.06594141768317741, -22.67126532539353789, 2.757051763020445634 ) ) ;
#5675 = CARTESIAN_POINT ( 'NONE',  ( -13.09030858231679417, -21.32581373872472597, 1.729004561291657582 ) ) ;
#5676 = ORIENTED_EDGE ( 'NONE', *, *, #10058, .F. ) ;
#5677 = CARTESIAN_POINT ( 'NONE',  ( 12.81251082758882376, -11.53070320674076576, 6.423537912489145185 ) ) ;
#5678 = CARTESIAN_POINT ( 'NONE',  ( 12.62503976493681535, -19.49799187068907713, 4.533161381885315144 ) ) ;
#5679 = VECTOR ( 'NONE', #9540, 1000.000000000000000 ) ;
#5680 = DIRECTION ( 'NONE',  ( 0.000000000000000000, 1.000000000000000000, 0.000000000000000000 ) ) ;
#5681 = VERTEX_POINT ( 'NONE', #4796 ) ;
#5682 = VERTEX_POINT ( 'NONE', #9296 ) ;
#5683 = CARTESIAN_POINT ( 'NONE',  ( -0.000000000000000000, 10.00000000000000000, 0.000000000000000000 ) ) ;
#5684 = VECTOR ( 'NONE', #18511, 1000.000000000000000 ) ;
#5685 = CYLINDRICAL_SURFACE ( 'NONE', #12904, 0.3750000000000003331 ) ;
#5686 = CARTESIAN_POINT ( 'NONE',  ( -24.87918902992234393, 10.00000000000000000, 0.000000000000000000 ) ) ;
#5687 = EDGE_CURVE ( 'NONE', #14757, #15085, #15671, .T. ) ;
#5688 = LINE ( 'NONE', #15505, #13056 ) ;
#5689 = CARTESIAN_POINT ( 'NONE',  ( 0.000000000000000000, -9.114917468222230923, 2.372643865078340575 ) ) ;
#5690 = CARTESIAN_POINT ( 'NONE',  ( 0.000000000000000000, 9.000000000000000000, 1.000000000000000000 ) ) ;
#5691 = CARTESIAN_POINT ( 'NONE',  ( 9.000000000000000000, -9.999999999999991118, 2.500000000000000000 ) ) ;
#5692 =( GEOMETRIC_REPRESENTATION_CONTEXT ( 3 ) GLOBAL_UNCERTAINTY_ASSIGNED_CONTEXT ( ( #15499 ) ) GLOBAL_UNIT_ASSIGNED_CONTEXT ( ( #19458, #505, #14416 ) ) REPRESENTATION_CONTEXT ( 'NONE', 'WORKASPACE' ) );
#5693 = CARTESIAN_POINT ( 'NONE',  ( -0.2815691515810352930, -9.114917468222230923, 2.372643865078523984 ) ) ;
#5694 = CARTESIAN_POINT ( 'NONE',  ( -9.340308582316795949, -22.98484643305508612, 6.020995438708344416 ) ) ;
#5695 = CARTESIAN_POINT ( 'NONE',  ( -1.513434189748285696, -9.114917468222230923, 1.622643865078341463 ) ) ;
#5696 = EDGE_LOOP ( 'NONE', ( #19728, #5782, #6765, #6254 ) ) ;
#5697 = AXIS2_PLACEMENT_3D ( 'NONE', #7347, #20216, #19910 ) ;
#5698 = CARTESIAN_POINT ( 'NONE',  ( -13.37499999999998401, -19.49999999999998934, 2.439580858552613751 ) ) ;
#5699 = CARTESIAN_POINT ( 'NONE',  ( -7.371558582316794173, -20.24999999999999289, 3.449312527122348371 ) ) ;
#5700 = CIRCLE ( 'NONE', #18725, 2.999999999999999112 ) ;
#5701 = EDGE_CURVE ( 'NONE', #20045, #4642, #20604, .T. ) ;
#5702 = CARTESIAN_POINT ( 'NONE',  ( 9.347191417683177406, -20.91377862118959285, 1.020995438708345082 ) ) ;
#5703 = CARTESIAN_POINT ( 'NONE',  ( -8.409691417683177406, -21.63647391050456648, 4.520995438708348857 ) ) ;
#5704 = ORIENTED_EDGE ( 'NONE', *, *, #18453, .F. ) ;
#5705 = EDGE_CURVE ( 'NONE', #16350, #6813, #1551, .T. ) ;
#5706 = CARTESIAN_POINT ( 'NONE',  ( 13.37561105820882013, -20.21914156045197686, 4.753815841436231260 ) ) ;
#5707 = DIRECTION ( 'NONE',  ( -1.156482317317871133E-15, -1.000000000000000000, 0.000000000000000000 ) ) ;
#5708 = ORIENTED_EDGE ( 'NONE', *, *, #14971, .F. ) ;
#5709 = ORIENTED_EDGE ( 'NONE', *, *, #3165, .F. ) ;
#5710 = DIRECTION ( 'NONE',  ( 0.000000000000000000, -1.000000000000000000, 0.000000000000000000 ) ) ;
#5711 = VERTEX_POINT ( 'NONE', #15876 ) ;
#5712 = CARTESIAN_POINT ( 'NONE',  ( -13.49014615398506045, -14.43511922376608680, 5.596513032956658584 ) ) ;
#5713 = ORIENTED_EDGE ( 'NONE', *, *, #11261, .F. ) ;
#5714 = AXIS2_PLACEMENT_3D ( 'NONE', #8743, #1105, #7483 ) ;
#5715 = DIRECTION ( 'NONE',  ( 0.000000000000000000, -1.000000000000000000, 0.000000000000000000 ) ) ;
#5716 = ADVANCED_FACE ( 'NONE', ( #15976 ), #4893, .T. ) ;
#5717 = FACE_OUTER_BOUND ( 'NONE', #15828, .T. ) ;
#5718 = VECTOR ( 'NONE', #6845, 1000.000000000000000 ) ;
#5719 = VECTOR ( 'NONE', #19388, 1000.000000000000000 ) ;
#5720 = DIRECTION ( 'NONE',  ( 0.000000000000000000, -1.000000000000000000, 0.000000000000000000 ) ) ;
#5721 = CARTESIAN_POINT ( 'NONE',  ( 1.643076795806035717, -8.364903549957356077, 2.372640290589878909 ) ) ;
#5722 = LINE ( 'NONE', #1120, #2512 ) ;
#5723 = CARTESIAN_POINT ( 'NONE',  ( 13.87372783958217681, 4.185755898898970706, 6.732634959205082481 ) ) ;
#5724 = CARTESIAN_POINT ( 'NONE',  ( -5.000000000000000000, -7.500000000000000000, 3.160254037844365094 ) ) ;
#5725 = CARTESIAN_POINT ( 'NONE',  ( 26.04469207716615031, 0.000000000000000000, 0.000000000000000000 ) ) ;
#5726 = DIRECTION ( 'NONE',  ( 0.000000000000000000, 0.000000000000000000, 1.000000000000000000 ) ) ;
#5727 = CARTESIAN_POINT ( 'NONE',  ( 4.003441417683176518, -22.05068747287765873, 5.250000000000000888 ) ) ;
#5728 = CARTESIAN_POINT ( 'NONE',  ( -12.62599079447150885, -20.19996487918709249, 4.820256282269618886 ) ) ;
#5729 = CARTESIAN_POINT ( 'NONE',  ( -9.534691417683177406, -20.97900456129164581, 3.136473910504570917 ) ) ;
#5730 = CIRCLE ( 'NONE', #10417, 0.3749999999999997224 ) ;
#5731 = CARTESIAN_POINT ( 'NONE',  ( -8.690941417683177406, -23.80360840875937001, 5.231925497173365081 ) ) ;
#5732 = VERTEX_POINT ( 'NONE', #4490 ) ;
#5733 = CARTESIAN_POINT ( 'NONE',  ( 12.62500000000002132, -19.49999999999450040, 3.833333333368183382 ) ) ;
#5734 = CARTESIAN_POINT ( 'NONE',  ( -12.68288333306630378, -17.32689168014509207, 5.548858176248425700 ) ) ;
#5735 = VERTEX_POINT ( 'NONE', #1456 ) ;
#5736 = VECTOR ( 'NONE', #20135, 1000.000000000000000 ) ;
#5737 = FACE_OUTER_BOUND ( 'NONE', #16733, .T. ) ;
#5738 = CARTESIAN_POINT ( 'NONE',  ( -15.87779268661489773, 0.000000000000000000, 1.000000000000000000 ) ) ;
#5739 = ORIENTED_EDGE ( 'NONE', *, *, #11586, .F. ) ;
#5740 = VERTEX_POINT ( 'NONE', #7835 ) ;
#5741 = ORIENTED_EDGE ( 'NONE', *, *, #17813, .F. ) ;
#5742 = CARTESIAN_POINT ( 'NONE',  ( 20.00000000000000000, -5.999999999999994671, 1.000000000000000000 ) ) ;
#5743 = ADVANCED_FACE ( 'NONE', ( #1658 ), #6256, .F. ) ;
#5744 = DIRECTION ( 'NONE',  ( -1.000000000000000000, 0.000000000000000000, 0.000000000000000000 ) ) ;
#5745 = CARTESIAN_POINT ( 'NONE',  ( -1.513434189748285696, -9.114917468222230923, 1.622643865078341463 ) ) ;
#5746 = CARTESIAN_POINT ( 'NONE',  ( 25.54469207716615031, 0.000000000000000000, 1.000000000000000000 ) ) ;
#5747 = LINE ( 'NONE', #1449, #18093 ) ;
#5748 = VECTOR ( 'NONE', #6643, 1000.000000000000000 ) ;
#5749 = CARTESIAN_POINT ( 'NONE',  ( 1.937849085826861328, 10.00000000000000000, 1.000000000000000000 ) ) ;
#5750 = CARTESIAN_POINT ( 'NONE',  ( 12.34719141768317741, -20.91377862118959285, 1.020995438708345082 ) ) ;
#5751 = CARTESIAN_POINT ( 'NONE',  ( -13.10557919622060652, 4.019249409169220577, 6.007898877577752650 ) ) ;
#5752 = CARTESIAN_POINT ( 'NONE',  ( -8.128441417683177406, -19.49999999999998934, 3.550687472877664952 ) ) ;
#5753 = ORIENTED_EDGE ( 'NONE', *, *, #13835, .T. ) ;
#5754 = LINE ( 'NONE', #8989, #3945 ) ;
#5755 = CARTESIAN_POINT ( 'NONE',  ( -17.94064177244175795, 11.64110105645932691, 0.000000000000000000 ) ) ;
#5756 = CARTESIAN_POINT ( 'NONE',  ( -13.39995901559228031, -19.73956971259024229, 6.178279423016713956 ) ) ;
#5757 = CARTESIAN_POINT ( 'NONE',  ( 10.65280858231679240, -21.22443879296942626, 5.229004561291659137 ) ) ;
#5758 = PLANE ( 'NONE',  #8322 ) ;
#5759 = ORIENTED_EDGE ( 'NONE', *, *, #4302, .T. ) ;
#5760 = ORIENTED_EDGE ( 'NONE', *, *, #15250, .T. ) ;
#5761 = CARTESIAN_POINT ( 'NONE',  ( 13.37526900345969771, -20.98641532528209908, 4.724331462949078464 ) ) ;
#5762 = CARTESIAN_POINT ( 'NONE',  ( -10.38119784648305632, -14.00000000000000000, 2.000000000000000000 ) ) ;
#5763 = ORIENTED_EDGE ( 'NONE', *, *, #14331, .T. ) ;
#5764 = AXIS2_PLACEMENT_3D ( 'NONE', #6543, #7901, #11047 ) ;
#5765 = CARTESIAN_POINT ( 'NONE',  ( 15.00000000000000355, -5.999999999999996447, 2.000000000000000000 ) ) ;
#5766 = PLANE ( 'NONE',  #16708 ) ;
#5767 = CARTESIAN_POINT ( 'NONE',  ( -9.715308582316794173, -23.77099543870833998, 2.825813738724734847 ) ) ;
#5768 = LINE ( 'NONE', #7641, #18282 ) ;
#5769 = CARTESIAN_POINT ( 'NONE',  ( -7.500000000000000888, -9.999999999999992895, 2.000000000000000000 ) ) ;
#5770 = CARTESIAN_POINT ( 'NONE',  ( 2.830107938415192148, -10.43856789473369950, 1.962583737180462418 ) ) ;
#5771 = ADVANCED_FACE ( 'NONE', ( #11080 ), #3892, .F. ) ;
#5772 = LINE ( 'NONE', #952, #15728 ) ;
#5773 = CARTESIAN_POINT ( 'NONE',  ( -13.09560264576187905, 4.265433610975056133, 4.333333333333380999 ) ) ;
#5774 = CARTESIAN_POINT ( 'NONE',  ( 0.000000000000000000, 4.999999999999999112, 1.000000000000000000 ) ) ;
#5775 = CARTESIAN_POINT ( 'NONE',  ( -13.41175265982446696, -19.14399067886409256, 6.245281310864100988 ) ) ;
#5776 = AXIS2_PLACEMENT_3D ( 'NONE', #2202, #437, #19795 ) ;
#5777 = FACE_OUTER_BOUND ( 'NONE', #15242, .T. ) ;
#5778 = CARTESIAN_POINT ( 'NONE',  ( 6.059058582316795949, -21.25705176302045274, 4.171265325393551215 ) ) ;
#5779 = EDGE_CURVE ( 'NONE', #16197, #20119, #13406, .T. ) ;
#5780 = CARTESIAN_POINT ( 'NONE',  ( 12.34719141768317741, -21.53509896474923835, 2.520995438708346192 ) ) ;
#5781 = CARTESIAN_POINT ( 'NONE',  ( -12.15280858231679595, -21.22443879296942626, 5.229004561291659137 ) ) ;
#5782 = ORIENTED_EDGE ( 'NONE', *, *, #4200, .F. ) ;
#5783 = CARTESIAN_POINT ( 'NONE',  ( 13.09080647246885576, 4.023226859705822278, 5.257958009367514229 ) ) ;
#5784 = CARTESIAN_POINT ( 'NONE',  ( -7.369520639128046113, 4.999999999999999112, 0.000000000000000000 ) ) ;
#5785 = ORIENTED_EDGE ( 'NONE', *, *, #8063, .T. ) ;
#5786 = ORIENTED_EDGE ( 'NONE', *, *, #13749, .T. ) ;
#5787 = CARTESIAN_POINT ( 'NONE',  ( -11.99999999999999467, -17.50000000000000000, 4.000000000000000000 ) ) ;
#5788 = VECTOR ( 'NONE', #15988, 1000.000000000000000 ) ;
#5789 = CARTESIAN_POINT ( 'NONE',  ( -12.72125031657057015, -15.38935901321805133, 5.590524842915047365 ) ) ;
#5790 = CARTESIAN_POINT ( 'NONE',  ( -2.659620708751979645, -10.38426118526329489, 2.698636689302993830 ) ) ;
#5791 = CARTESIAN_POINT ( 'NONE',  ( -13.85980676119184629, 4.232741440188380722, 5.965367510457697975 ) ) ;
#5792 = ADVANCED_FACE ( 'NONE', ( #7700 ), #617, .T. ) ;
#5793 = CARTESIAN_POINT ( 'NONE',  ( 15.00000000000001421, -25.49999999999999645, 4.000000000000000000 ) ) ;
#5794 = DIRECTION ( 'NONE',  ( 1.000000000000000000, 0.000000000000000000, 0.000000000000000000 ) ) ;
#5795 = LINE ( 'NONE', #9235, #10838 ) ;
#5796 = DIRECTION ( 'NONE',  ( 0.000000000000000000, -0.000000000000000000, 1.000000000000000000 ) ) ;
#5797 = CARTESIAN_POINT ( 'NONE',  ( -1.407845757905374695, -9.114917468222230923, 2.372643865078341019 ) ) ;
#5798 = CARTESIAN_POINT ( 'NONE',  ( -12.15280858231679950, -20.91377862118960351, 5.979004561291660913 ) ) ;
#5799 = CARTESIAN_POINT ( 'NONE',  ( -2.682825141213236009, -9.727160171598653093, 1.779880022082258373 ) ) ;
#5800 = ORIENTED_EDGE ( 'NONE', *, *, #11830, .F. ) ;
#5801 = CARTESIAN_POINT ( 'NONE',  ( -13.38449802415168932, -19.02034978033825396, 4.747874963382372471 ) ) ;
#5802 = DIRECTION ( 'NONE',  ( -0.000000000000000000, -0.000000000000000000, -1.000000000000000000 ) ) ;
#5803 = CARTESIAN_POINT ( 'NONE',  ( 11.78469141768317741, -24.52099543870834708, 4.484846433055073689 ) ) ;
#5804 = CARTESIAN_POINT ( 'NONE',  ( -12.06594141768317741, -22.67126532539353789, 2.757051763020445634 ) ) ;
#5805 = EDGE_LOOP ( 'NONE', ( #12151, #15573, #2353, #1057 ) ) ;
#5806 = CARTESIAN_POINT ( 'NONE',  ( 13.47096266223369376, -15.40388555723029462, 5.575679699623145247 ) ) ;
#5807 = DIRECTION ( 'NONE',  ( 1.000000000000000000, 0.000000000000000000, 0.000000000000000000 ) ) ;
#5808 = ORIENTED_EDGE ( 'NONE', *, *, #15862, .F. ) ;
#5809 = EDGE_CURVE ( 'NONE', #12435, #4874, #2789, .T. ) ;
#5810 = VERTEX_POINT ( 'NONE', #18898 ) ;
#5811 = DIRECTION ( 'NONE',  ( 0.000000000000000000, 1.000000000000000000, -0.000000000000000000 ) ) ;
#5812 = ORIENTED_EDGE ( 'NONE', *, *, #15869, .F. ) ;
#5813 = CARTESIAN_POINT ( 'NONE',  ( -13.41341218697771609, -18.31018455762212227, 5.513179699623425023 ) ) ;
#5814 = VECTOR ( 'NONE', #8832, 1000.000000000000000 ) ;
#5815 = CARTESIAN_POINT ( 'NONE',  ( 2.559937518207947793, -9.746075135043517079, 2.534737762559237773 ) ) ;
#5816 = VERTEX_POINT ( 'NONE', #2393 ) ;
#5817 = CARTESIAN_POINT ( 'NONE',  ( -27.49999999999999645, -4.770489558936219510E-14, 0.000000000000000000 ) ) ;
#5818 = LINE ( 'NONE', #9061, #14336 ) ;
#5819 = EDGE_CURVE ( 'NONE', #15395, #3029, #19775, .T. ) ;
#5820 = ADVANCED_FACE ( 'NONE', ( #3860 ), #8783, .T. ) ;
#5821 = CARTESIAN_POINT ( 'NONE',  ( 7.499999999999999112, -18.49999999999999645, 6.500000000000000888 ) ) ;
#5822 = CARTESIAN_POINT ( 'NONE',  ( 0.000000000000000000, -8.364917468222230923, 2.372643865078341019 ) ) ;
#5823 = DIRECTION ( 'NONE',  ( 2.312964634635752916E-15, 1.000000000000000000, -0.000000000000000000 ) ) ;
#5824 = CARTESIAN_POINT ( 'NONE',  ( 12.66503773474750894, -18.97809439524806052, 6.263381662489337920 ) ) ;
#5825 = DIRECTION ( 'NONE',  ( -0.000000000000000000, -0.000000000000000000, -1.000000000000000000 ) ) ;
#5826 = CARTESIAN_POINT ( 'NONE',  ( 11.00000000000000000, -25.49999999999999645, 6.500000000000000000 ) ) ;
#5827 = CARTESIAN_POINT ( 'NONE',  ( 4.750698171653723989, 10.00000000000000000, 0.000000000000000000 ) ) ;
#5828 = CARTESIAN_POINT ( 'NONE',  ( 10.94094141768317741, -21.25705176302044208, 2.828734674606458555 ) ) ;
#5829 = DIRECTION ( 'NONE',  ( 0.000000000000000000, -0.000000000000000000, -1.000000000000000000 ) ) ;
#5830 = CARTESIAN_POINT ( 'NONE',  ( -11.02780858231679595, -22.97900456129165647, 3.964901035250747885 ) ) ;
#5831 = CARTESIAN_POINT ( 'NONE',  ( -8.409691417683177406, -21.01515356694492098, 6.020995438708349745 ) ) ;
#5832 = ORIENTED_EDGE ( 'NONE', *, *, #6586, .T. ) ;
#5833 = CARTESIAN_POINT ( 'NONE',  ( 12.62499999999998224, -19.50000000000006040, 4.416666666666682062 ) ) ;
#5834 = CARTESIAN_POINT ( 'NONE',  ( -13.10012427866737639, 3.743776072700027324, 6.001983176248468332 ) ) ;
#5835 = ORIENTED_EDGE ( 'NONE', *, *, #4163, .T. ) ;
#5836 = EDGE_CURVE ( 'NONE', #15932, #8657, #8673, .T. ) ;
#5837 = LINE ( 'NONE', #17015, #18317 ) ;
#5838 = DIRECTION ( 'NONE',  ( 1.000000000000000000, 0.000000000000000000, -0.000000000000000000 ) ) ;
#5839 = ORIENTED_EDGE ( 'NONE', *, *, #2732, .F. ) ;
#5840 = CARTESIAN_POINT ( 'NONE',  ( 2.623717082130370137, -10.12934627674766830, 2.633169448359191644 ) ) ;
#5841 = ORIENTED_EDGE ( 'NONE', *, *, #15509, .T. ) ;
#5842 = ORIENTED_EDGE ( 'NONE', *, *, #1216, .T. ) ;
#5843 = CARTESIAN_POINT ( 'NONE',  ( 4.750698171653723989, 0.000000000000000000, 1.000000000000000000 ) ) ;
#5844 = CARTESIAN_POINT ( 'NONE',  ( -14.49999999999998579, -24.49999999999999289, 4.000000000000000000 ) ) ;
#5845 = EDGE_CURVE ( 'NONE', #14133, #13753, #1220, .T. ) ;
#5846 = EDGE_CURVE ( 'NONE', #9650, #1231, #20262, .T. ) ;
#5847 = CARTESIAN_POINT ( 'NONE',  ( -2.340131407102140848, -12.21153219924485889, 2.225301406344140531 ) ) ;
#5848 = LINE ( 'NONE', #12732, #2691 ) ;
#5849 = PLANE ( 'NONE',  #7959 ) ;
#5850 = CARTESIAN_POINT ( 'NONE',  ( 25.37918902992234393, 16.00000000000000000, 1.000000000000000000 ) ) ;
#5851 = CARTESIAN_POINT ( 'NONE',  ( 11.59719141768317741, -23.08622137881040359, 5.979004561291654696 ) ) ;
#5852 = CARTESIAN_POINT ( 'NONE',  ( -13.10821839766814279, 4.152529082241303904, 5.997503362667785609 ) ) ;
#5853 = CARTESIAN_POINT ( 'NONE',  ( -8.690941417683177406, -23.80360840875937001, 5.231925497173365081 ) ) ;
#5854 = ORIENTED_EDGE ( 'NONE', *, *, #4678, .T. ) ;
#5855 = CARTESIAN_POINT ( 'NONE',  ( 12.52780858231679595, -23.72900456129165647, 4.275561207030568411 ) ) ;
#5856 = FACE_OUTER_BOUND ( 'NONE', #3698, .T. ) ;
#5857 = CARTESIAN_POINT ( 'NONE',  ( -13.38172782443493602, -20.66024486603417643, 5.557997437521964734 ) ) ;
#5858 = EDGE_CURVE ( 'NONE', #7250, #13818, #9368, .T. ) ;
#5859 = CARTESIAN_POINT ( 'NONE',  ( 11.12155858231679417, -23.74999999999999645, 3.550687472877651629 ) ) ;
#5860 = DIRECTION ( 'NONE',  ( -1.000000000000000000, 0.000000000000000000, 0.000000000000000000 ) ) ;
#5861 = ORIENTED_EDGE ( 'NONE', *, *, #14349, .T. ) ;
#5862 = ORIENTED_EDGE ( 'NONE', *, *, #7858, .F. ) ;
#5863 = CARTESIAN_POINT ( 'NONE',  ( 13.37499999999998401, -20.99999999999999645, 3.146526952850934755 ) ) ;
#5864 = LINE ( 'NONE', #16937, #13915 ) ;
#5865 = ORIENTED_EDGE ( 'NONE', *, *, #8911, .F. ) ;
#5866 = DIRECTION ( 'NONE',  ( -0.4999999999999947264, -0.8660254037844417052, 0.000000000000000000 ) ) ;
#5867 = ORIENTED_EDGE ( 'NONE', *, *, #1874, .F. ) ;
#5868 = CARTESIAN_POINT ( 'NONE',  ( -10.84030858231679240, -22.67418626127525982, 5.270995438708342640 ) ) ;
#5869 = DIRECTION ( 'NONE',  ( -0.000000000000000000, -0.000000000000000000, -1.000000000000000000 ) ) ;
#5870 = CARTESIAN_POINT ( 'NONE',  ( 13.12529397354238192, 5.014845663890297622, 3.999999999999981792 ) ) ;
#5871 = CARTESIAN_POINT ( 'NONE',  ( 2.226467333542268445, -8.440126719678968215, 1.641959103308203716 ) ) ;
#5872 = DIRECTION ( 'NONE',  ( 0.000000000000000000, 1.000000000000000000, -0.000000000000000000 ) ) ;
#5873 = CARTESIAN_POINT ( 'NONE',  ( -13.09560264576187905, 4.265433610975056133, 4.666666666666618113 ) ) ;
#5874 = VECTOR ( 'NONE', #17221, 1000.000000000000000 ) ;
#5875 = DIRECTION ( 'NONE',  ( -4.625929269271486111E-15, -1.000000000000000000, 0.000000000000000000 ) ) ;
#5876 = CARTESIAN_POINT ( 'NONE',  ( -13.83079205777725917, 2.017498917744843023, 6.700359435863729729 ) ) ;
#5877 = CARTESIAN_POINT ( 'NONE',  ( 0.000000000000000000, 11.64110105645932691, 10.00000000000000000 ) ) ;
#5878 = CARTESIAN_POINT ( 'NONE',  ( 12.99655858231679417, -22.05068747287764452, 1.749999999999998446 ) ) ;
#5879 = CARTESIAN_POINT ( 'NONE',  ( 10.19094141768317741, -22.74294823697955081, 4.171265325393542334 ) ) ;
#5880 = CARTESIAN_POINT ( 'NONE',  ( -12.34030858231679240, -22.67418626127525982, 5.270995438708342640 ) ) ;
#5881 = ORIENTED_EDGE ( 'NONE', *, *, #1798, .F. ) ;
#5882 = CARTESIAN_POINT ( 'NONE',  ( 13.09560264576187905, 4.265433610975056133, 4.833333333333343695 ) ) ;
#5883 = DIRECTION ( 'NONE',  ( 0.000000000000000000, 0.000000000000000000, 1.000000000000000000 ) ) ;
#5884 = ORIENTED_EDGE ( 'NONE', *, *, #14507, .T. ) ;
#5885 = EDGE_CURVE ( 'NONE', #610, #2607, #14168, .T. ) ;
#5886 = ORIENTED_EDGE ( 'NONE', *, *, #8574, .F. ) ;
#5887 = DIRECTION ( 'NONE',  ( 0.000000000000000000, 0.000000000000000000, 1.000000000000000000 ) ) ;
#5888 = CARTESIAN_POINT ( 'NONE',  ( -13.09293046926041626, 3.380488697651010011, 5.994170676248444352 ) ) ;
#5889 = CARTESIAN_POINT ( 'NONE',  ( -2.567175533087980188, -9.771398394011347577, 2.541241281345096859 ) ) ;
#5890 = CARTESIAN_POINT ( 'NONE',  ( -13.39359219590679295, -19.31109410670777038, 5.491647114909025795 ) ) ;
#5891 = CARTESIAN_POINT ( 'NONE',  ( 0.000000000000000000, 4.999999999999999112, 1.000000000000000000 ) ) ;
#5892 = DIRECTION ( 'NONE',  ( 0.000000000000000000, -0.000000000000000000, 1.000000000000000000 ) ) ;
#5893 = CARTESIAN_POINT ( 'NONE',  ( -11.00000000000000000, -20.16506350946107418, 5.250000000000000000 ) ) ;
#5894 = PLANE ( 'NONE',  #18096 ) ;
#5895 = CARTESIAN_POINT ( 'NONE',  ( -9.999999999999996447, -34.99999999999999289, 1.000000000000000000 ) ) ;
#5896 = CARTESIAN_POINT ( 'NONE',  ( -9.809058582316795949, -23.80360840875935935, 1.768074502826626260 ) ) ;
#5897 = CARTESIAN_POINT ( 'NONE',  ( -2.916276642307554123, -11.05036367517186058, 2.119705115445599475 ) ) ;
#5898 = VERTEX_POINT ( 'NONE', #6445 ) ;
#5899 = CARTESIAN_POINT ( 'NONE',  ( -13.83890698502169059, 3.927302743594121903, 5.241364546715693074 ) ) ;
#5900 = FACE_OUTER_BOUND ( 'NONE', #9664, .T. ) ;
#5901 = CARTESIAN_POINT ( 'NONE',  ( 11.69094141768317741, -23.80360840875937001, 5.231925497173365081 ) ) ;
#5902 = CARTESIAN_POINT ( 'NONE',  ( -7.565941417683177406, -22.67126532539353789, 2.757051763020445634 ) ) ;
#5903 = VERTEX_POINT ( 'NONE', #2992 ) ;
#5904 = CARTESIAN_POINT ( 'NONE',  ( 13.40787921250184311, -19.33959976865745389, 6.241060671539915283 ) ) ;
#5905 = LINE ( 'NONE', #12584, #20422 ) ;
#5906 = ORIENTED_EDGE ( 'NONE', *, *, #5288, .F. ) ;
#5907 = ORIENTED_EDGE ( 'NONE', *, *, #14210, .T. ) ;
#5908 = CARTESIAN_POINT ( 'NONE',  ( 13.50000000000001243, -19.49999999999999645, 1.000000000000000000 ) ) ;
#5909 = EDGE_CURVE ( 'NONE', #18372, #18307, #13418, .T. ) ;
#5910 = ORIENTED_EDGE ( 'NONE', *, *, #15898, .F. ) ;
#5911 = CARTESIAN_POINT ( 'NONE',  ( -13.87467358130843387, 4.983515856073828409, 5.065827972856573602 ) ) ;
#5912 = CARTESIAN_POINT ( 'NONE',  ( -14.00147952833368770, -0.02431694168600004660, 0.6777495337877021964 ) ) ;
#5913 = EDGE_CURVE ( 'NONE', #20101, #12443, #13014, .T. ) ;
#5914 = EDGE_CURVE ( 'NONE', #15986, #2296, #19415, .T. ) ;
#5915 = ORIENTED_EDGE ( 'NONE', *, *, #11787, .T. ) ;
#5916 = DIRECTION ( 'NONE',  ( 0.000000000000000000, -0.000000000000000000, 1.000000000000000000 ) ) ;
#5917 = CARTESIAN_POINT ( 'NONE',  ( 23.31633994409548549, 10.00000000000000000, 1.000000000000000000 ) ) ;
#5918 = CARTESIAN_POINT ( 'NONE',  ( -7.869520639128047002, 0.000000000000000000, 1.000000000000000000 ) ) ;
#5919 = CARTESIAN_POINT ( 'NONE',  ( 2.532303758294933704, -8.551221675625164664, 1.670490507339845054 ) ) ;
#5920 = CARTESIAN_POINT ( 'NONE',  ( 0.000000000000000000, 10.00000000000000000, 1.000000000000000000 ) ) ;
#5921 = CARTESIAN_POINT ( 'NONE',  ( 5.000000000000000000, -7.500000000000000000, 1.000000000000000000 ) ) ;
#5922 = DIRECTION ( 'NONE',  ( -0.000000000000000000, -0.000000000000000000, -1.000000000000000000 ) ) ;
#5923 = DIRECTION ( 'NONE',  ( 0.000000000000000000, -1.000000000000000000, 0.000000000000000000 ) ) ;
#5924 = CARTESIAN_POINT ( 'NONE',  ( 15.36404127825609400, 9.000000000000001776, 0.000000000000000000 ) ) ;
#5925 = CARTESIAN_POINT ( 'NONE',  ( 6.159691417683175629, -22.36352608949543352, 2.479004561291652031 ) ) ;
#5926 = CARTESIAN_POINT ( 'NONE',  ( -13.11017182064853159, 4.251176942750957366, 5.979809059808775196 ) ) ;
#5927 = CARTESIAN_POINT ( 'NONE',  ( -7.652808582316796837, -21.53509896474924901, 4.479004561291659137 ) ) ;
#5928 = CARTESIAN_POINT ( 'NONE',  ( -7.565941417683177406, -23.73192549717336064, 1.696391591240623331 ) ) ;
#5929 = VERTEX_POINT ( 'NONE', #3400 ) ;
#5930 = CARTESIAN_POINT ( 'NONE',  ( 13.12463908936614132, 4.981774012991869505, 5.264611377988129171 ) ) ;
#5931 = CARTESIAN_POINT ( 'NONE',  ( -13.11017182064853159, 4.251176942750957366, 5.979809059808775196 ) ) ;
#5932 = ORIENTED_EDGE ( 'NONE', *, *, #12798, .T. ) ;
#5933 = VECTOR ( 'NONE', #24, 1000.000000000000000 ) ;
#5934 = DIRECTION ( 'NONE',  ( -0.000000000000000000, -0.000000000000000000, -1.000000000000000000 ) ) ;
#5935 = ADVANCED_FACE ( 'NONE', ( #4761 ), #17421, .T. ) ;
#5936 = ORIENTED_EDGE ( 'NONE', *, *, #11266, .T. ) ;
#5937 = CARTESIAN_POINT ( 'NONE',  ( 1.866357130655357688, -10.00562759449716133, 2.408781036472938730 ) ) ;
#5938 = ORIENTED_EDGE ( 'NONE', *, *, #281, .T. ) ;
#5939 = LINE ( 'NONE', #13669, #20356 ) ;
#5940 = DIRECTION ( 'NONE',  ( 0.000000000000000000, 1.000000000000000000, -0.000000000000000000 ) ) ;
#5941 = CARTESIAN_POINT ( 'NONE',  ( -2.124709647372160060, -10.68204274815009924, 1.832497960681391147 ) ) ;
#5942 = FACE_OUTER_BOUND ( 'NONE', #16393, .T. ) ;
#5943 = DIRECTION ( 'NONE',  ( -1.000000000000000000, 0.000000000000000000, 0.000000000000000000 ) ) ;
#5944 = EDGE_CURVE ( 'NONE', #12925, #4929, #59, .T. ) ;
#5945 = DIRECTION ( 'NONE',  ( 4.625929269271477434E-15, 1.000000000000000000, 0.000000000000000000 ) ) ;
#5946 = CARTESIAN_POINT ( 'NONE',  ( 11.22219141768317741, -19.52099543870834353, 4.586221378810406257 ) ) ;
#5947 = CARTESIAN_POINT ( 'NONE',  ( -13.12503131243110843, 5.001581277770153378, 5.166347330538456184 ) ) ;
#5948 = CARTESIAN_POINT ( 'NONE',  ( -8.034691417683175629, -20.22900456129164581, 2.825813738724747726 ) ) ;
#5949 = ORIENTED_EDGE ( 'NONE', *, *, #9322, .T. ) ;
#5950 = CARTESIAN_POINT ( 'NONE',  ( 10.93405858231679417, -23.20159541128345992, 4.773278322869455970 ) ) ;
#5951 = DIRECTION ( 'NONE',  ( 0.000000000000000000, 0.000000000000000000, -1.000000000000000000 ) ) ;
#5952 = CARTESIAN_POINT ( 'NONE',  ( -13.37543017851028893, -20.97827598523083026, 4.780017688621249761 ) ) ;
#5953 = VERTEX_POINT ( 'NONE', #15743 ) ;
#5954 = CARTESIAN_POINT ( 'NONE',  ( 5.777808582316795949, -21.02099543870833998, 3.035098964749253003 ) ) ;
#5955 = EDGE_CURVE ( 'NONE', #1443, #20090, #14264, .T. ) ;
#5956 = DIRECTION ( 'NONE',  ( 1.000000000000000000, 0.000000000000000000, 0.000000000000000000 ) ) ;
#5957 = VERTEX_POINT ( 'NONE', #12809 ) ;
#5958 = EDGE_CURVE ( 'NONE', #932, #19920, #9472, .T. ) ;
#5959 = ORIENTED_EDGE ( 'NONE', *, *, #13196, .T. ) ;
#5960 = CARTESIAN_POINT ( 'NONE',  ( 13.40957725085194241, -19.25384883197511243, 6.242932005802575901 ) ) ;
#5961 = DIRECTION ( 'NONE',  ( 1.000000000000000000, 2.312964634635756072E-15, 0.000000000000000000 ) ) ;
#5962 = ORIENTED_EDGE ( 'NONE', *, *, #16707, .T. ) ;
#5963 = VECTOR ( 'NONE', #15228, 1000.000000000000000 ) ;
#5964 = CARTESIAN_POINT ( 'NONE',  ( -11.74178095869206828, 0.000000000000000000, 1.000000000000000000 ) ) ;
#5965 = VECTOR ( 'NONE', #17002, 1000.000000000000000 ) ;
#5966 = VERTEX_POINT ( 'NONE', #16058 ) ;
#5967 = CARTESIAN_POINT ( 'NONE',  ( -11.21530858231679417, -23.77099543870833998, 2.825813738724734847 ) ) ;
#5968 = PLANE ( 'NONE',  #5583 ) ;
#5969 = VECTOR ( 'NONE', #9488, 1000.000000000000000 ) ;
#5970 = CARTESIAN_POINT ( 'NONE',  ( 20.00000000000000000, 3.000000000000004441, 1.000000000000000000 ) ) ;
#5971 = CARTESIAN_POINT ( 'NONE',  ( 3.232228556578340850, -13.29361487011126464, 2.695816835751057461 ) ) ;
#5972 = CARTESIAN_POINT ( 'NONE',  ( 14.50000000000001243, -18.49999999999999645, 4.000000000000000000 ) ) ;
#5973 = CARTESIAN_POINT ( 'NONE',  ( -13.09560264576187905, 4.265433610975056133, 2.999999999999999556 ) ) ;
#5974 = VECTOR ( 'NONE', #12160, 1000.000000000000000 ) ;
#5975 = AXIS2_PLACEMENT_3D ( 'NONE', #12728, #3315, #14089 ) ;
#5976 = CARTESIAN_POINT ( 'NONE',  ( 10.93405858231679417, -23.20159541128345992, 4.773278322869455970 ) ) ;
#5977 = CARTESIAN_POINT ( 'NONE',  ( -13.37499999998404299, -20.99999999996810729, 2.793053905886972998 ) ) ;
#5978 = VECTOR ( 'NONE', #11552, 1000.000000000000000 ) ;
#5979 = DIRECTION ( 'NONE',  ( 0.000000000000000000, 0.000000000000000000, 1.000000000000000000 ) ) ;
#5980 = CARTESIAN_POINT ( 'NONE',  ( 12.34030858231679240, -22.67418626127525982, 5.270995438708342640 ) ) ;
#5981 = CARTESIAN_POINT ( 'NONE',  ( 4.565941417683176518, -23.20159541128344927, 2.226721677130534705 ) ) ;
#5982 = CARTESIAN_POINT ( 'NONE',  ( -5.590308582316794173, -21.32581373872472597, 1.729004561291657582 ) ) ;
#5983 = ORIENTED_EDGE ( 'NONE', *, *, #19115, .T. ) ;
#5984 = CARTESIAN_POINT ( 'NONE',  ( 13.09543520949579865, 4.256978079540234106, 5.067654010725516578 ) ) ;
#5985 = CARTESIAN_POINT ( 'NONE',  ( -0.9854920305337621089, -9.114917468222230923, 1.622643865078341463 ) ) ;
#5986 = ORIENTED_EDGE ( 'NONE', *, *, #4238, .T. ) ;
#5987 = ORIENTED_EDGE ( 'NONE', *, *, #1253, .T. ) ;
#5988 = CARTESIAN_POINT ( 'NONE',  ( 12.00000000000000178, -26.50000000000000355, 1.000000000000000000 ) ) ;
#5989 = VECTOR ( 'NONE', #5374, 1000.000000000000000 ) ;
#5990 = VECTOR ( 'NONE', #489, 1000.000000000000000 ) ;
#5991 = CARTESIAN_POINT ( 'NONE',  ( -12.63943061533661982, -19.52125392549825733, 5.470334935344855154 ) ) ;
#5992 = VECTOR ( 'NONE', #7099, 1000.000000000000000 ) ;
#5993 = CARTESIAN_POINT ( 'NONE',  ( -2.109407804498405703, -9.207748739546751438, 2.396484790045401603 ) ) ;
#5994 = CARTESIAN_POINT ( 'NONE',  ( -13.87406079471522347, 4.952570133121557028, 5.260711232101737522 ) ) ;
#5995 = EDGE_CURVE ( 'NONE', #15113, #14620, #14436, .T. ) ;
#5996 = CYLINDRICAL_SURFACE ( 'NONE', #5312, 10.00000000000000000 ) ;
#5997 = DIRECTION ( 'NONE',  ( 0.000000000000000000, -1.000000000000000000, 0.000000000000000000 ) ) ;
#5998 = CARTESIAN_POINT ( 'NONE',  ( 5.381197846483058989, -14.00000000000000000, 2.000000000000000000 ) ) ;
#5999 = DIRECTION ( 'NONE',  ( 0.000000000000000000, 0.000000000000000000, 1.000000000000000000 ) ) ;
#6000 = CARTESIAN_POINT ( 'NONE',  ( -1.126276606324276619, -9.114917468222230923, 2.372643865078341019 ) ) ;
#6001 = CARTESIAN_POINT ( 'NONE',  ( -7.840308582316795949, -22.98484643305508612, 6.020995438708344416 ) ) ;
#6002 = CARTESIAN_POINT ( 'NONE',  ( -2.627360420079438263, -14.25085146736906339, 2.749039333894452763 ) ) ;
#6003 = VERTEX_POINT ( 'NONE', #3196 ) ;
#6004 = CARTESIAN_POINT ( 'NONE',  ( -13.84485691484488257, 4.227774199669918964, 5.063753864839139140 ) ) ;
#6005 = PLANE ( 'NONE',  #8390 ) ;
#6006 = CARTESIAN_POINT ( 'NONE',  ( 11.03469141768317741, -19.47900456129164581, 2.515153566944927199 ) ) ;
#6007 = CARTESIAN_POINT ( 'NONE',  ( -13.09030858231679417, -21.63647391050454871, 2.479004561291657804 ) ) ;
#6008 = VECTOR ( 'NONE', #4747, 1000.000000000000000 ) ;
#6009 = ORIENTED_EDGE ( 'NONE', *, *, #821, .F. ) ;
#6010 = CARTESIAN_POINT ( 'NONE',  ( 13.86693669322925260, 4.592803008081209448, 5.801483467520450077 ) ) ;
#6011 = CARTESIAN_POINT ( 'NONE',  ( 21.67243175760212637, 0.000000000000000000, 0.000000000000000000 ) ) ;
#6012 = VECTOR ( 'NONE', #9267, 1000.000000000000000 ) ;
#6013 = ORIENTED_EDGE ( 'NONE', *, *, #6264, .T. ) ;
#6014 = VERTEX_POINT ( 'NONE', #1424 ) ;
#6015 = DIRECTION ( 'NONE',  ( -0.000000000000000000, -0.000000000000000000, -1.000000000000000000 ) ) ;
#6016 = VECTOR ( 'NONE', #6753, 1000.000000000000000 ) ;
#6017 = ORIENTED_EDGE ( 'NONE', *, *, #18921, .F. ) ;
#6018 = DIRECTION ( 'NONE',  ( 0.000000000000000000, 1.000000000000000000, 0.000000000000000000 ) ) ;
#6019 = DIRECTION ( 'NONE',  ( 1.000000000000000000, 0.000000000000000000, 0.000000000000000000 ) ) ;
#6020 = VERTEX_POINT ( 'NONE', #7806 ) ;
#6021 = CARTESIAN_POINT ( 'NONE',  ( 10.38119784648305810, -14.00000000000000000, 1.000000000000000000 ) ) ;
#6022 = CARTESIAN_POINT ( 'NONE',  ( 3.277163086644854229, -14.76879761173520578, 3.824673233536266537 ) ) ;
#6023 = VECTOR ( 'NONE', #17027, 1000.000000000000000 ) ;
#6024 = VECTOR ( 'NONE', #19484, 1000.000000000000000 ) ;
#6025 = LINE ( 'NONE', #13857, #7337 ) ;
#6026 = CARTESIAN_POINT ( 'NONE',  ( 1.852280067228949445, -9.126254559850970338, 1.625555456689752321 ) ) ;
#6027 = DIRECTION ( 'NONE',  ( -0.000000000000000000, -0.000000000000000000, -1.000000000000000000 ) ) ;
#6028 = CARTESIAN_POINT ( 'NONE',  ( 13.11145189917479392, 4.315820908324673688, 5.961432613039677086 ) ) ;
#6029 = VECTOR ( 'NONE', #777, 1000.000000000000000 ) ;
#6030 = EDGE_CURVE ( 'NONE', #15705, #175, #12905, .T. ) ;
#6031 = DIRECTION ( 'NONE',  ( 1.000000000000000000, -0.000000000000000000, 0.000000000000000000 ) ) ;
#6032 = DIRECTION ( 'NONE',  ( 0.000000000000000000, 0.000000000000000000, -1.000000000000000000 ) ) ;
#6033 = CARTESIAN_POINT ( 'NONE',  ( 27.94203811574922725, 3.231447299068595019E-14, 1.000000000000000000 ) ) ;
#6034 = CARTESIAN_POINT ( 'NONE',  ( 13.18405858231679595, -21.32873467460644079, 2.757051763020455404 ) ) ;
#6035 = CARTESIAN_POINT ( 'NONE',  ( -13.10624331898488037, 4.052787608736739600, 6.006964772046813117 ) ) ;
#6036 = CARTESIAN_POINT ( 'NONE',  ( -8.027808582316795949, -22.97900456129165647, 3.964901035250747885 ) ) ;
#6037 = CARTESIAN_POINT ( 'NONE',  ( -5.222191417683177406, -19.52099543870834353, 4.586221378810406257 ) ) ;
#6038 = VERTEX_POINT ( 'NONE', #16166 ) ;
#6039 = EDGE_CURVE ( 'NONE', #9021, #9247, #9568, .T. ) ;
#6040 = CARTESIAN_POINT ( 'NONE',  ( 13.06641424290328501, 2.791419266617020334, 5.231470106674447784 ) ) ;
#6041 = DIRECTION ( 'NONE',  ( 0.000000000000000000, 0.000000000000000000, -1.000000000000000000 ) ) ;
#6042 = ORIENTED_EDGE ( 'NONE', *, *, #1798, .T. ) ;
#6043 = EDGE_CURVE ( 'NONE', #8463, #6462, #6227, .T. ) ;
#6044 = FACE_OUTER_BOUND ( 'NONE', #1210, .T. ) ;
#6045 = SHAPE_REPRESENTATION ( 'spring', ( #18039 ), #12033 ) ;
#6046 = ORIENTED_EDGE ( 'NONE', *, *, #1849, .T. ) ;
#6047 = CARTESIAN_POINT ( 'NONE',  ( 2.594671182134835163, -9.923034775318452461, 2.580184533305832861 ) ) ;
#6048 = VECTOR ( 'NONE', #1843, 1000.000000000000000 ) ;
#6049 = AXIS2_PLACEMENT_3D ( 'NONE', #15825, #9652, #17712 ) ;
#6050 = VECTOR ( 'NONE', #16534, 1000.000000000000000 ) ;
#6051 = VERTEX_POINT ( 'NONE', #14372 ) ;
#6052 = LINE ( 'NONE', #14088, #3976 ) ;
#6053 = PLANE ( 'NONE',  #10282 ) ;
#6054 = CARTESIAN_POINT ( 'NONE',  ( -1.665360951492234287, -9.864914341757378580, 1.622643062139706993 ) ) ;
#6055 = PLANE ( 'NONE',  #14705 ) ;
#6056 = DIRECTION ( 'NONE',  ( 0.000000000000000000, 0.2487476929738665354, 0.9685683172808094987 ) ) ;
#6057 = EDGE_CURVE ( 'NONE', #18629, #12851, #11344, .T. ) ;
#6058 = DIRECTION ( 'NONE',  ( -1.000000000000000000, 0.000000000000000000, 0.000000000000000000 ) ) ;
#6059 = CARTESIAN_POINT ( 'NONE',  ( 4.190941417683176518, -23.80360840875937001, 5.231925497173365081 ) ) ;
#6060 = PRESENTATION_STYLE_ASSIGNMENT (( #1247 ) ) ;
#6061 = CARTESIAN_POINT ( 'NONE',  ( -11.97219141768317563, -23.72900456129165292, 2.724438792969417822 ) ) ;
#6062 = VECTOR ( 'NONE', #17811, 1000.000000000000000 ) ;
#6063 = ORIENTED_EDGE ( 'NONE', *, *, #16145, .F. ) ;
#6064 = CARTESIAN_POINT ( 'NONE',  ( 10.09030858231679595, -21.32581373872472597, 1.729004561291657582 ) ) ;
#6065 = DIRECTION ( 'NONE',  ( 0.000000000000000000, 0.1264857625231113059, -0.9919684228235025047 ) ) ;
#6066 = CARTESIAN_POINT ( 'NONE',  ( -12.66204031416134335, -19.12946413485185104, 6.260126454156002218 ) ) ;
#6067 = ORIENTED_EDGE ( 'NONE', *, *, #3902, .F. ) ;
#6068 = CARTESIAN_POINT ( 'NONE',  ( 4.840308582316793284, -22.67418626127525982, 5.270995438708342640 ) ) ;
#6069 = FACE_OUTER_BOUND ( 'NONE', #17969, .T. ) ;
#6070 = ORIENTED_EDGE ( 'NONE', *, *, #17734, .F. ) ;
#6071 = ORIENTED_EDGE ( 'NONE', *, *, #6527, .T. ) ;
#6072 = CARTESIAN_POINT ( 'NONE',  ( 13.37499999999998224, -20.99999999999998934, 4.291666666666699825 ) ) ;
#6073 = CARTESIAN_POINT ( 'NONE',  ( 5.683390479346035029, 9.000000000000001776, 1.000000000000000000 ) ) ;
#6074 = ORIENTED_EDGE ( 'NONE', *, *, #10792, .F. ) ;
#6075 = ADVANCED_FACE ( 'NONE', ( #11241 ), #12598, .T. ) ;
#6076 = DIRECTION ( 'NONE',  ( -0.000000000000000000, -0.000000000000000000, -1.000000000000000000 ) ) ;
#6077 = ORIENTED_EDGE ( 'NONE', *, *, #448, .T. ) ;
#6078 = CARTESIAN_POINT ( 'NONE',  ( -9.434058582316794173, -23.20159541128345992, 4.773278322869455970 ) ) ;
#6079 = VECTOR ( 'NONE', #17889, 1000.000000000000000 ) ;
#6080 = CARTESIAN_POINT ( 'NONE',  ( -5.381197846483055436, -14.00000000000000000, 2.000000000000000000 ) ) ;
#6081 = CARTESIAN_POINT ( 'NONE',  ( 11.00000000000000000, -20.16506350946107418, 5.250000000000000000 ) ) ;
#6082 = CARTESIAN_POINT ( 'NONE',  ( 1.639793706121975614, -8.364901960018411131, 1.622639882261793343 ) ) ;
#6083 = ADVANCED_FACE ( 'NONE', ( #9672 ), #12704, .T. ) ;
#6084 = EDGE_CURVE ( 'NONE', #20035, #6794, #12923, .T. ) ;
#6085 = CARTESIAN_POINT ( 'NONE',  ( 16.37779268661489596, 10.00000000000000000, 1.000000000000000000 ) ) ;
#6086 = CARTESIAN_POINT ( 'NONE',  ( -13.37499999999998224, -19.49999999999991473, 4.333333333333343695 ) ) ;
#6087 = CARTESIAN_POINT ( 'NONE',  ( 5.027808582316793284, -23.72900456129165647, 4.275561207030568411 ) ) ;
#6088 = CARTESIAN_POINT ( 'NONE',  ( -12.62505438222622622, -20.99725369757571869, 4.613400783263607252 ) ) ;
#6089 = CARTESIAN_POINT ( 'NONE',  ( -13.17791111847408025, 4.999999999999999112, 1.000000000000000000 ) ) ;
#6090 = CARTESIAN_POINT ( 'NONE',  ( 6.715308582316796837, -23.02099543870833998, 3.136473910504556262 ) ) ;
#6091 = VECTOR ( 'NONE', #16158, 1000.000000000000114 ) ;
#6092 = CARTESIAN_POINT ( 'NONE',  ( 10.84719141768317741, -21.53509896474923835, 2.520995438708346192 ) ) ;
#6093 = CARTESIAN_POINT ( 'NONE',  ( -5.871558582316794173, -20.24999999999999289, 3.449312527122348371 ) ) ;
#6094 = ORIENTED_EDGE ( 'NONE', *, *, #18843, .F. ) ;
#6095 = CARTESIAN_POINT ( 'NONE',  ( 13.09559422631463654, 4.265008428887424152, 5.017082219073495608 ) ) ;
#6096 = FACE_OUTER_BOUND ( 'NONE', #4573, .T. ) ;
#6097 = VERTEX_POINT ( 'NONE', #17636 ) ;
#6098 = ORIENTED_EDGE ( 'NONE', *, *, #14680, .T. ) ;
#6099 = CARTESIAN_POINT ( 'NONE',  ( 15.00000000000001421, -29.99999999999998579, 1.000000000000000000 ) ) ;
#6100 = CARTESIAN_POINT ( 'NONE',  ( -13.00900269284621302, -0.8578640112522492034, 5.903024842915844062 ) ) ;
#6101 = CARTESIAN_POINT ( 'NONE',  ( -0.5631383031621635116, -8.364917468222230923, 2.372643865078341019 ) ) ;
#6102 = CARTESIAN_POINT ( 'NONE',  ( -13.87467358130843387, 4.983515856073828409, 5.065827972856573602 ) ) ;
#6103 = AXIS2_PLACEMENT_3D ( 'NONE', #2531, #18449, #16863 ) ;
#6104 = EDGE_CURVE ( 'NONE', #15422, #49, #77, .T. ) ;
#6105 = LINE ( 'NONE', #20331, #9388 ) ;
#6106 = DIRECTION ( 'NONE',  ( 0.000000000000000000, -1.000000000000000000, 0.000000000000000000 ) ) ;
#6107 = LINE ( 'NONE', #17595, #12360 ) ;
#6108 = CARTESIAN_POINT ( 'NONE',  ( -20.00349085826861995, 10.00000000000000000, 1.000000000000000000 ) ) ;
#6109 = CARTESIAN_POINT ( 'NONE',  ( -11.40280858231679595, -23.08622137881038938, 1.020995438708339309 ) ) ;
#6110 = CARTESIAN_POINT ( 'NONE',  ( -2.195822829018478473, -9.226849102155203042, 1.651390144731336163 ) ) ;
#6111 = ORIENTED_EDGE ( 'NONE', *, *, #2536, .F. ) ;
#6112 = CARTESIAN_POINT ( 'NONE',  ( -13.82811627091129836, 3.382371681020614584, 5.229645796715683304 ) ) ;
#6113 = CARTESIAN_POINT ( 'NONE',  ( 7.499999999999999112, -23.70993649053891517, 5.466506350946108483 ) ) ;
#6114 = CARTESIAN_POINT ( 'NONE',  ( 12.06594141768317741, -23.73192549717336064, 1.696391591240623331 ) ) ;
#6115 = CARTESIAN_POINT ( 'NONE',  ( -11.96530858231679773, -20.97900456129165647, 3.863526089495444626 ) ) ;
#6116 = VERTEX_POINT ( 'NONE', #4982 ) ;
#6117 = CARTESIAN_POINT ( 'NONE',  ( 13.87066368810231154, 4.781016249162736820, 5.617237349937618696 ) ) ;
#6118 = CARTESIAN_POINT ( 'NONE',  ( -18.69064177244175795, 10.00000000000000000, 1.000000000000000000 ) ) ;
#6119 = EDGE_LOOP ( 'NONE', ( #4229, #2375, #18773, #17453 ) ) ;
#6120 = ORIENTED_EDGE ( 'NONE', *, *, #16252, .T. ) ;
#6121 = AXIS2_PLACEMENT_3D ( 'NONE', #17048, #7227, #1262 ) ;
#6122 = ADVANCED_FACE ( 'NONE', ( #19435 ), #11257, .T. ) ;
#6123 = CARTESIAN_POINT ( 'NONE',  ( 1.937849085826861328, 0.000000000000000000, 0.000000000000000000 ) ) ;
#6124 = ORIENTED_EDGE ( 'NONE', *, *, #11640, .T. ) ;
#6125 = CARTESIAN_POINT ( 'NONE',  ( -13.54769662923970763, -11.52882022337116119, 5.659013032956382361 ) ) ;
#6126 = CARTESIAN_POINT ( 'NONE',  ( 1.717920576997000737, -9.114924032904250240, 2.372645551019823884 ) ) ;
#6127 = ORIENTED_EDGE ( 'NONE', *, *, #6722, .F. ) ;
#6128 = CARTESIAN_POINT ( 'NONE',  ( -24.50000000000000000, 0.000000000000000000, 1.000000000000000000 ) ) ;
#6129 = CARTESIAN_POINT ( 'NONE',  ( 4.999999999999998224, -2.500000000000047518, 9.999999999999998224 ) ) ;
#6130 = CARTESIAN_POINT ( 'NONE',  ( -20.49999999999998224, -21.99999999999999645, 11.00000000000000178 ) ) ;
#6131 = CARTESIAN_POINT ( 'NONE',  ( 1.819865260185086875, -9.122006307963404836, 1.624464420737683046 ) ) ;
#6132 = DIRECTION ( 'NONE',  ( -0.000000000000000000, 0.000000000000000000, -1.000000000000000000 ) ) ;
#6133 = CARTESIAN_POINT ( 'NONE',  ( 13.10252221513633941, 3.864871864382954048, 6.004587342915129966 ) ) ;
#6134 = CARTESIAN_POINT ( 'NONE',  ( 3.999999999999999112, -7.500000000000047073, 9.999999999999998224 ) ) ;
#6135 = LINE ( 'NONE', #10741, #1042 ) ;
#6136 = DIRECTION ( 'NONE',  ( 0.000000000000000000, -1.000000000000000000, 0.000000000000000000 ) ) ;
#6137 = CARTESIAN_POINT ( 'NONE',  ( 8.034691417683175629, -20.97900456129164581, 3.136473910504570917 ) ) ;
#6138 = CARTESIAN_POINT ( 'NONE',  ( -12.64751377014909828, -19.11305460747000495, 5.510446717915143289 ) ) ;
#6139 = CARTESIAN_POINT ( 'NONE',  ( -12.80905858231679417, -22.74294823697954016, 2.828734674606448785 ) ) ;
#6140 = CARTESIAN_POINT ( 'NONE',  ( -5.409691417683178294, -21.01515356694492098, 6.020995438708349745 ) ) ;
#6141 = EDGE_LOOP ( 'NONE', ( #19348, #6633, #13061, #5210, #8102, #216 ) ) ;
#6142 = CARTESIAN_POINT ( 'NONE',  ( 13.09543520949579865, 4.256978079540234106, 5.067654010725516578 ) ) ;
#6143 = CYLINDRICAL_SURFACE ( 'NONE', #7548, 10.00000000000000000 ) ;
#6144 = ORIENTED_EDGE ( 'NONE', *, *, #10117, .F. ) ;
#6145 = CARTESIAN_POINT ( 'NONE',  ( -10.43924542913431175, 0.000000000000000000, 1.000000000000000000 ) ) ;
#6146 = CIRCLE ( 'NONE', #2753, 10.00000000000000000 ) ;
#6147 = VERTEX_POINT ( 'NONE', #9490 ) ;
#6148 = CARTESIAN_POINT ( 'NONE',  ( 1.716273078461125090, -9.866787073280026021, 2.373124017006284170 ) ) ;
#6149 = VECTOR ( 'NONE', #15582, 1000.000000000000000 ) ;
#6150 = ADVANCED_FACE ( 'NONE', ( #12826 ), #15858, .F. ) ;
#6151 = APPLICATION_CONTEXT ( 'automotive_design' ) ;
#6152 = VERTEX_POINT ( 'NONE', #3113 ) ;
#6153 = DIRECTION ( 'NONE',  ( 1.000000000000000000, 0.000000000000000000, 0.000000000000000000 ) ) ;
#6154 = DIRECTION ( 'NONE',  ( -0.1351665943404259662, -0.9596796555888893465, 0.2464649070825324084 ) ) ;
#6155 = CARTESIAN_POINT ( 'NONE',  ( -2.196516900615978152, -11.19187256518208784, 1.963432442569047698 ) ) ;
#6156 = PLANE ( 'NONE',  #19684 ) ;
#6157 = CARTESIAN_POINT ( 'NONE',  ( -9.305650798910056309, 9.000000000000001776, 1.000000000000000000 ) ) ;
#6158 = CARTESIAN_POINT ( 'NONE',  ( -20.00349085826861995, 0.000000000000000000, 1.000000000000000000 ) ) ;
#6159 = CARTESIAN_POINT ( 'NONE',  ( 9.065941417683177406, -23.73192549717336064, 1.696391591240623331 ) ) ;
#6160 = CARTESIAN_POINT ( 'NONE',  ( -10.37844141768317741, -23.74999999999999645, 3.449312527122335492 ) ) ;
#6161 = SHAPE_REPRESENTATION ( 'spring housing', ( #18039 ), #15032 ) ;
#6162 = ORIENTED_EDGE ( 'NONE', *, *, #15196, .F. ) ;
#6163 = CARTESIAN_POINT ( 'NONE',  ( 5.027808582316793284, -23.72900456129165647, 4.275561207030568411 ) ) ;
#6164 = CARTESIAN_POINT ( 'NONE',  ( 11.00000000000000000, -20.29006350946107418, 5.466506350946110260 ) ) ;
#6165 = CARTESIAN_POINT ( 'NONE',  ( -12.62499999999998401, -20.99999999999999645, 3.666666666666654084 ) ) ;
#6166 = CARTESIAN_POINT ( 'NONE',  ( 7.277808582316794173, -20.27099543870833642, 2.724438792969431589 ) ) ;
#6167 = PLANE ( 'NONE',  #7325 ) ;
#6168 = ORIENTED_EDGE ( 'NONE', *, *, #16852, .T. ) ;
#6169 = FACE_OUTER_BOUND ( 'NONE', #17436, .T. ) ;
#6170 = EDGE_LOOP ( 'NONE', ( #1413, #18671, #4643, #13388, #3461, #19865, #5808, #7585, #14855, #14050, #2585, #8182 ) ) ;
#6171 = EDGE_CURVE ( 'NONE', #42, #7093, #16766, .T. ) ;
#6172 = CARTESIAN_POINT ( 'NONE',  ( 9.000000000000000000, -9.999999999999991118, 1.000000000000000000 ) ) ;
#6173 = ORIENTED_EDGE ( 'NONE', *, *, #19115, .F. ) ;
#6174 = CARTESIAN_POINT ( 'NONE',  ( -10.46530858231679417, -20.22900456129164937, 4.174186261275266929 ) ) ;
#6175 = CARTESIAN_POINT ( 'NONE',  ( 12.64195242771744709, -19.39390240027112000, 5.496549442168085164 ) ) ;
#6176 = ADVANCED_FACE ( 'NONE', ( #17751 ), #9897, .T. ) ;
#6177 = DIRECTION ( 'NONE',  ( -1.000000000000000000, 0.000000000000000000, 0.000000000000000000 ) ) ;
#6178 = CARTESIAN_POINT ( 'NONE',  ( 3.506783328160878010, -9.991161114504492957, 2.040295720924476530 ) ) ;
#6179 = ADVANCED_FACE ( 'NONE', ( #9691 ), #4879, .F. ) ;
#6180 = CARTESIAN_POINT ( 'NONE',  ( 0.000000000000000000, 9.000000000000001776, 1.000000000000000000 ) ) ;
#6181 = CARTESIAN_POINT ( 'NONE',  ( -13.37500751150753864, -19.49962066887028556, 4.515663405036051792 ) ) ;
#6182 = CARTESIAN_POINT ( 'NONE',  ( 7.277808582316794173, -20.27099543870833642, 2.724438792969431589 ) ) ;
#6183 = CARTESIAN_POINT ( 'NONE',  ( -12.62499999999998401, -20.99999999999999645, 3.666666666666654084 ) ) ;
#6184 = LINE ( 'NONE', #14323, #4704 ) ;
#6185 = CARTESIAN_POINT ( 'NONE',  ( 5.590308582316794173, -21.32581373872472597, 1.729004561291657582 ) ) ;
#6186 = CARTESIAN_POINT ( 'NONE',  ( 6.347191417683176518, -21.53509896474923835, 2.520995438708346192 ) ) ;
#6187 = CARTESIAN_POINT ( 'NONE',  ( -11.69094141768317563, -23.27327832286946219, 4.701595411283453707 ) ) ;
#6188 = ORIENTED_EDGE ( 'NONE', *, *, #1772, .T. ) ;
#6189 = CARTESIAN_POINT ( 'NONE',  ( 13.57153706873194032, -9.574878029060977624, 4.950999963380944280 ) ) ;
#6190 = CARTESIAN_POINT ( 'NONE',  ( -1.754777266914451461, -9.116337928146160507, 1.623008667563337726 ) ) ;
#6191 = ORIENTED_EDGE ( 'NONE', *, *, #6746, .F. ) ;
#6192 = ADVANCED_FACE ( 'NONE', ( #14281 ), #20690, .T. ) ;
#6193 = ORIENTED_EDGE ( 'NONE', *, *, #11641, .F. ) ;
#6194 = CARTESIAN_POINT ( 'NONE',  ( 0.000000000000000000, 4.999999999999999112, 1.000000000000000000 ) ) ;
#6195 = CARTESIAN_POINT ( 'NONE',  ( -4.000000000000000000, 0.000000000000000000, 0.000000000000000000 ) ) ;
#6196 = AXIS2_PLACEMENT_3D ( 'NONE', #13045, #17862, #1960 ) ;
#6197 = CARTESIAN_POINT ( 'NONE',  ( -3.537356407578672535, -11.36437789272258669, 3.142965222332344766 ) ) ;
#6198 = CARTESIAN_POINT ( 'NONE',  ( -13.39542766346049518, -19.21840299524461315, 5.493648449623241170 ) ) ;
#6199 = CARTESIAN_POINT ( 'NONE',  ( 8.876396343307449754, 10.00000000000000000, 1.000000000000000000 ) ) ;
#6200 = LINE ( 'NONE', #2959, #13539 ) ;
#6201 = CARTESIAN_POINT ( 'NONE',  ( 13.09030858231679417, -21.32581373872472952, 1.729004561291657138 ) ) ;
#6202 = DIRECTION ( 'NONE',  ( -1.000000000000000000, 0.000000000000000000, 0.000000000000000000 ) ) ;
#6203 = CARTESIAN_POINT ( 'NONE',  ( 13.12035191997235906, 4.015271958632619764, 6.757839745787993735 ) ) ;
#6204 = CARTESIAN_POINT ( 'NONE',  ( -6.996558582316795949, -22.05068747287764452, 0.9999999999999978906 ) ) ;
#6205 = CARTESIAN_POINT ( 'NONE',  ( -1.744064896197293324, -9.868721669903177229, 1.623620860066563365 ) ) ;
#6206 = VERTEX_POINT ( 'NONE', #13033 ) ;
#6207 = CARTESIAN_POINT ( 'NONE',  ( -13.84501465882535598, 4.235740270674679842, 5.020612255068622076 ) ) ;
#6208 = LINE ( 'NONE', #9244, #8716 ) ;
#6209 = CARTESIAN_POINT ( 'NONE',  ( 5.597191417683177406, -23.08622137881040359, 5.979004561291654696 ) ) ;
#6210 = CARTESIAN_POINT ( 'NONE',  ( -12.71530858231679417, -23.02099543870833998, 3.136473910504556262 ) ) ;
#6211 = ORIENTED_EDGE ( 'NONE', *, *, #7357, .T. ) ;
#6212 = CARTESIAN_POINT ( 'NONE',  ( 13.37499999999998224, -20.99999999999998934, 4.166666666666637653 ) ) ;
#6213 = DIRECTION ( 'NONE',  ( 0.000000000000000000, -1.000000000000000000, 0.000000000000000000 ) ) ;
#6214 = DIRECTION ( 'NONE',  ( -0.000000000000000000, -0.000000000000000000, -1.000000000000000000 ) ) ;
#6215 = ORIENTED_EDGE ( 'NONE', *, *, #15799, .F. ) ;
#6216 = EDGE_CURVE ( 'NONE', #14649, #17557, #9797, .T. ) ;
#6217 = ORIENTED_EDGE ( 'NONE', *, *, #4755, .F. ) ;
#6218 = EDGE_CURVE ( 'NONE', #7096, #14361, #12722, .T. ) ;
#6219 = LINE ( 'NONE', #14254, #10783 ) ;
#6220 = CARTESIAN_POINT ( 'NONE',  ( -13.98883902916702482, -0.1144964390440934426, 0.8305393671244342135 ) ) ;
#6221 = ORIENTED_EDGE ( 'NONE', *, *, #11418, .T. ) ;
#6222 = LINE ( 'NONE', #6128, #12195 ) ;
#6223 = CARTESIAN_POINT ( 'NONE',  ( -15.87779268661489773, 11.64110105645932691, 0.000000000000000000 ) ) ;
#6224 = CARTESIAN_POINT ( 'NONE',  ( -11.75209451496117197, 16.00000000000000000, 1.000000000000000000 ) ) ;
#6225 = CARTESIAN_POINT ( 'NONE',  ( 1.652577328807104839, -9.114908150887895744, 1.622641472200749835 ) ) ;
#6226 = CARTESIAN_POINT ( 'NONE',  ( 10.05565079891005631, 0.000000000000000000, 1.000000000000000000 ) ) ;
#6227 = LINE ( 'NONE', #19207, #86 ) ;
#6228 = ADVANCED_FACE ( 'NONE', ( #8133 ), #16078, .T. ) ;
#6229 = CARTESIAN_POINT ( 'NONE',  ( -4.000000000000000000, -8.500000000000000000, 2.392927049865408495 ) ) ;
#6230 = DIRECTION ( 'NONE',  ( -0.000000000000000000, -0.000000000000000000, -1.000000000000000000 ) ) ;
#6231 = CARTESIAN_POINT ( 'NONE',  ( -3.047379876266447685, -13.13734219723468755, 3.405682891496055742 ) ) ;
#6232 = CARTESIAN_POINT ( 'NONE',  ( 4.659691417683177406, -22.36352608949543352, 2.479004561291652031 ) ) ;
#6233 = CARTESIAN_POINT ( 'NONE',  ( -12.62500000000002132, -19.49999999999450040, 3.833333333368183382 ) ) ;
#6234 = CARTESIAN_POINT ( 'NONE',  ( -11.77780858231679595, -21.02099543870833998, 3.035098964749253003 ) ) ;
#6235 = CARTESIAN_POINT ( 'NONE',  ( -7.097191417683176518, -23.08622137881040359, 5.979004561291654696 ) ) ;
#6236 = ORIENTED_EDGE ( 'NONE', *, *, #17554, .F. ) ;
#6237 = CARTESIAN_POINT ( 'NONE',  ( 13.08559773465513487, 3.760185600081874746, 5.252303440007609403 ) ) ;
#6238 = CARTESIAN_POINT ( 'NONE',  ( 0.000000000000000000, 11.64110105645932691, 10.00000000000000000 ) ) ;
#6239 = VERTEX_POINT ( 'NONE', #1750 ) ;
#6240 = PLANE ( 'NONE',  #15650 ) ;
#6241 = EDGE_LOOP ( 'NONE', ( #5708, #1080, #10881, #4479 ) ) ;
#6242 = CARTESIAN_POINT ( 'NONE',  ( 2.579281110863027582, -9.822567596814183233, 2.554382554832406615 ) ) ;
#6243 = VERTEX_POINT ( 'NONE', #4779 ) ;
#6244 = CARTESIAN_POINT ( 'NONE',  ( 12.53469141768317741, -20.22900456129164581, 2.825813738724748170 ) ) ;
#6245 = PLANE ( 'NONE',  #3625 ) ;
#6246 = CARTESIAN_POINT ( 'NONE',  ( -1.857501949683560971, -9.975525523312803955, 2.401050223243493154 ) ) ;
#6247 = FACE_OUTER_BOUND ( 'NONE', #4344, .T. ) ;
#6248 = CARTESIAN_POINT ( 'NONE',  ( -10.55905858231679595, -20.72672167713054137, 4.701595411283463477 ) ) ;
#6249 = ADVANCED_FACE ( 'NONE', ( #11163 ), #17534, .T. ) ;
#6250 = DIRECTION ( 'NONE',  ( 0.000000000000000000, -1.000000000000000000, 0.000000000000000000 ) ) ;
#6251 = CARTESIAN_POINT ( 'NONE',  ( 9.159691417683175629, -22.98484643305507191, 0.9790045612916508100 ) ) ;
#6252 = FACE_OUTER_BOUND ( 'NONE', #9105, .T. ) ;
#6253 = CARTESIAN_POINT ( 'NONE',  ( -7.472191417683176518, -23.72900456129165292, 2.724438792969417822 ) ) ;
#6254 = ORIENTED_EDGE ( 'NONE', *, *, #17526, .T. ) ;
#6255 = CARTESIAN_POINT ( 'NONE',  ( 7.559058582316794173, -20.72672167713054137, 4.701595411283463477 ) ) ;
#6256 = PLANE ( 'NONE',  #17433 ) ;
#6257 = CARTESIAN_POINT ( 'NONE',  ( -13.90439735423812273, 5.734566389025032684, 3.666666666666500873 ) ) ;
#6258 = ORIENTED_EDGE ( 'NONE', *, *, #4317, .F. ) ;
#6259 = CIRCLE ( 'NONE', #17949, 10.00000000000000000 ) ;
#6260 = CARTESIAN_POINT ( 'NONE',  ( 6.996558582316793284, -22.05068747287764452, 1.749999999999998446 ) ) ;
#6261 = LINE ( 'NONE', #13897, #17332 ) ;
#6262 = APPLICATION_CONTEXT ( 'automotive_design' ) ;
#6263 = VERTEX_POINT ( 'NONE', #6559 ) ;
#6264 = EDGE_CURVE ( 'NONE', #15518, #5711, #9584, .T. ) ;
#6265 = FACE_OUTER_BOUND ( 'NONE', #2865, .T. ) ;
#6266 = ORIENTED_EDGE ( 'NONE', *, *, #9956, .F. ) ;
#6267 = FACE_OUTER_BOUND ( 'NONE', #14777, .T. ) ;
#6268 = ORIENTED_EDGE ( 'NONE', *, *, #310, .T. ) ;
#6269 = CARTESIAN_POINT ( 'NONE',  ( -5.309058582316794173, -23.27327832286945153, 2.298404588716537411 ) ) ;
#6270 = DIRECTION ( 'NONE',  ( 0.000000000000000000, 1.000000000000000000, 0.000000000000000000 ) ) ;
#6271 = DIRECTION ( 'NONE',  ( 0.000000000000000000, 1.000000000000000000, -0.000000000000000000 ) ) ;
#6272 = CARTESIAN_POINT ( 'NONE',  ( 1.126276606324276619, -9.114917468222230923, 1.622643865078341463 ) ) ;
#6273 = AXIS2_PLACEMENT_3D ( 'NONE', #1968, #404, #19454 ) ;
#6274 =( BOUNDED_SURFACE ( )  B_SPLINE_SURFACE ( 3, 3, ( 
 ( #7469, #12371, #18553, #4217, #4432, #1090, #13829, #10815, #12673, #17809, #9753, #19495, #4938, #1705, #17594, #9544, #17906, #16237, #15915, #6300, #19075, #6616, #16138, #3374, #5147, #229, #8400, #9643, #13092, #1592, #1804, #4732, #8190, #6519, #20643, #11525, #16029, #17490, #14556, #3170, #11318, #1903, #4837, #8089, #3573, #11120, #8286, #9852, #14345, #7972, #9952, #14660, #135, #16337, #29, #12882, #11424, #6416, #2011, #12781, #12988, #341, #19183, #6725, #11218, #3267, #14454, #19285, #17702, #19389, #5047, #3475, #18222, #7140, #2211, #20001, #10264, #12038, #10480, #3884, #19904, #4096, #13503, #11621, #3989, #13599 ),
 ( #14963, #19805, #16631, #2517, #18010, #18123, #3682, #10373, #8701, #753, #14767, #2312, #6920, #8496, #2418, #5559, #10066, #644, #16439, #7237, #444, #13289, #11930, #7032, #6823, #14866, #8809, #15072, #5460, #11832, #16747, #18432, #11731, #5667, #15178, #18324, #853, #16849, #13192, #19590, #5244, #3789, #2114, #16536, #541, #19690, #13399, #5353, #10166, #8593, #10993, #12453, #14017, #20213, #17363, #15385, #15692, #4298, #1068, #1377, #17058, #7447, #18534, #17162, #18745, #15276, #9214, #13810, #20426, #18848, #20110, #13910, #8908, #2838, #15585, #9116, #7755, #13705, #10580, #5873, #7547, #5773, #14122, #9013, #4509, #5973 ),
 ( #17257, #7645, #12144, #15485, #4197, #20527, #953, #12243, #6086, #1168, #20311, #16946, #6181, #7343, #2622, #1269, #10686, #2737, #18946, #10794, #12548, #9315, #10893, #2936, #12348, #18636, #4409, #4602, #17677, #7946, #12858, #5124, #14317, #15794, #209, #19260, #1883, #8066, #4817, #3, #12648, #313, #19362, #19054, #9425, #1474, #9729, #4914, #6497, #8264, #3349, #11504, #12758, #16215, #4711, #11291, #7852, #16113, #9617, #3050, #14630, #19161, #20623, #6593, #8168, #6392, #14215, #9520, #9830, #11194, #15892, #6699, #17571, #1572, #11099, #1781, #14534, #6276, #12961, #3243, #5019, #11399, #17470, #14429, #3147, #17784 ),
 ( #15998, #1677, #111, #3452, #13070, #19469, #9930, #13168, #14744, #16311, #420, #8370, #6800, #1983, #19568, #5221, #17884, #3551, #17179, #1393, #18551, #12260, #16967, #1287, #9134, #9335, #5890, #2645, #6198, #16866, #15504, #9231, #7667, #15711, #7564, #2535, #20546, #20130, #7776, #15403, #10705, #7467, #15602, #7363, #17078, #14139, #17273, #10595, #13928, #18653, #12566, #8925, #975, #4322, #15294, #18866, #2955, #18966, #4620, #12161, #13725, #2756, #12472, #5791, #1186, #14036, #4215, #20330, #9033, #1086, #5994, #2856, #20446, #6102, #13826, #20230, #12369, #4526, #18764, #4429, #10813, #10911, #15181, #13506, #10688, #857 ),
 ( #955, #5977, #7240, #7345, #12245, #16750, #18747, #17164, #1070, #17060, #13602, #2739, #2626, #12350, #1170, #9118, #7449, #20112, #2421, #10482, #13912, #15387, #5670, #10582, #2839, #12041, #19908, #18638, #16948, #20313, #5775, #2519, #18435, #10376, #4411, #15487, #8812, #7143, #5562, #13812, #9015, #4199, #10796, #20215, #9216, #16851, #756, #20005, #5876, #11933, #4301, #13707, #18327, #3992, #8910, #4098, #7550, #15278, #12146, #18536, #20529, #18850, #7854, #9318, #7648, #4819, #15694, #10895, #113, #11196, #15796, #6499, #1379, #1477, #6395, #17259, #12860, #11293, #15894, #17573, #7757, #3245, #4511, #2938, #17680, #3351 ),
 ( #14124, #8068, #3052, #6183, #12550, #3149, #4713, #1271, #1574, #18948, #5, #9619, #6088, #20625, #15587, #9522, #7948, #14218, #14432, #20428, #4604, #10996, #6278, #12455, #19262, #17365, #16002, #12652, #9427, #14320, #19056, #11101, #17472, #4916, #14020, #12760, #19163, #1679, #14942, #11401, #5126, #9832, #14843, #1986, #2188, #19472, #16217, #19778, #9731, #8373, #2092, #10038, #18200, #11506, #8572, #19365, #19570, #8170, #11601, #16313, #16116, #620, #17886, #6595, #5223, #12963, #423, #11703, #14632, #5021, #14746, #3454, #1783, #19666, #1885, #17786, #7007, #5329, #9933, #13375, #8266, #6802, #518, #317, #5436, #11809 ),
 ( #18100, #6701, #13072, #14536, #211, #3553, #17985, #3765, #13170, #3656, #8476, #16416, #6899, #13267, #10145, #16516, #7316, #8986, #13888, #16924, #731, #13787, #2710, #4271, #11907, #13576, #4072, #8884, #13677, #12320, #7115, #7214, #13478, #20192, #18513, #10555, #3863, #20084, #16720, #18297, #12221, #2598, #19881, #10458, #5537, #17032, #10240, #2396, #1039, #16827, #2491, #3960, #9092, #16606, #10348, #12121, #19978, #18408, #20289, #5751, #15462, #10658, #5852, #4173, #15253, #8786, #5639, #1147, #15359, #15155, #7425, #5947, #829, #2286, #18611, #7524, #8677, #929, #12012, #15046, #7620, #15972, #14292, #13989, #4385, #10768 ) ),
 .UNSPECIFIED., .T., .F., .F. ) 
 B_SPLINE_SURFACE_WITH_KNOTS ( ( 4, 3, 4 ),
 ( 4, 2, 2, 2, 2, 2, 2, 2, 2, 2, 2, 2, 2, 2, 2, 2, 2, 2, 2, 2, 2, 2, 2, 2, 2, 2, 2, 2, 2, 2, 2, 2, 2, 2, 2, 2, 2, 2, 2, 2, 2, 2, 4 ),
 ( 0.000000000000000000, 0.5000000000000000000, 1.000000000000000000 ),
 ( 0.000000000000000000, 0.03481082764294501225, 0.05122453910963481460, 0.05943139484297971231, 0.06353482270965216117, 0.06763825057632461002, 0.07081696859385246123, 0.07399568661138031245, 0.08035312264643601488, 0.09306799471654741973, 0.1057828667866588246, 0.1121403028217145270, 0.1153190208392423644, 0.1184977388567702156, 0.1214804596100246270, 0.1244631803632790246, 0.1304286218697878197, 0.1423595048828054099, 0.1662212709088405904, 0.2139448029609109514, 0.3093918670650516733, 0.5002859952733331728, 0.6911801234816146167, 0.7866271875857553386, 0.8343507196378256996, 0.8582124856638608801, 0.8701433686768784703, 0.8761088101833873765, 0.8790915309366418295, 0.8820742516898961716, 0.8853411830926052328, 0.8886081144953141830, 0.8951419773007323055, 0.9082097029115685505, 0.9212774285224047954, 0.9278112913278229179, 0.9310782227305318681, 0.9343451541332409294, 0.9384485819999133227, 0.9425520098665858271, 0.9507588655999306138, 0.9671725770666204092, 1.000000000000000000 ),
 .UNSPECIFIED. ) 
 GEOMETRIC_REPRESENTATION_ITEM ( )  RATIONAL_B_SPLINE_SURFACE ( (
 ( 1.000000000000000000, 1.000000000000000000, 1.000000000000000000, 1.000000000000000000, 1.000000000000000000, 1.000000000000000000, 1.000000000000000000, 1.000000000000000000, 1.000000000000000000, 1.000000000000000000, 1.000000000000000000, 1.000000000000000000, 1.000000000000000000, 1.000000000000000000, 1.000000000000000000, 1.000000000000000000, 1.000000000000000000, 1.000000000000000000, 1.000000000000000000, 1.000000000000000000, 1.000000000000000000, 1.000000000000000000, 1.000000000000000000, 1.000000000000000000, 1.000000000000000000, 1.000000000000000000, 1.000000000000000000, 1.000000000000000000, 1.000000000000000000, 1.000000000000000000, 1.000000000000000000, 1.000000000000000000, 1.000000000000000000, 1.000000000000000000, 1.000000000000000000, 1.000000000000000000, 1.000000000000000000, 1.000000000000000000, 1.000000000000000000, 1.000000000000000000, 1.000000000000000000, 1.000000000000000000, 1.000000000000000000, 1.000000000000000000, 1.000000000000000000, 1.000000000000000000, 1.000000000000000000, 1.000000000000000000, 1.000000000000000000, 1.000000000000000000, 1.000000000000000000, 1.000000000000000000, 1.000000000000000000, 1.000000000000000000, 1.000000000000000000, 1.000000000000000000, 1.000000000000000000, 1.000000000000000000, 1.000000000000000000, 1.000000000000000000, 1.000000000000000000, 1.000000000000000000, 1.000000000000000000, 1.000000000000000000, 1.000000000000000000, 1.000000000000000000, 1.000000000000000000, 1.000000000000000000, 1.000000000000000000, 1.000000000000000000, 1.000000000000000000, 1.000000000000000000, 1.000000000000000000, 1.000000000000000000, 1.000000000000000000, 1.000000000000000000, 1.000000000000000000, 1.000000000000000000, 1.000000000000000000, 1.000000000000000000, 1.000000000000000000, 1.000000000000000000, 1.000000000000000000, 1.000000000000000000, 1.000000000000000000, 1.000000000000000000),
 ( 0.3333333333333333703, 0.3333333333333333703, 0.3333333333333333703, 0.3333333333333333703, 0.3333333333333333703, 0.3333333333333333703, 0.3333333333333333703, 0.3333333333333333703, 0.3333333333333333703, 0.3333333333333333703, 0.3333333333333333703, 0.3333333333333333703, 0.3333333333333333703, 0.3333333333333333703, 0.3333333333333333703, 0.3333333333333333703, 0.3333333333333333703, 0.3333333333333333703, 0.3333333333333333703, 0.3333333333333333703, 0.3333333333333333703, 0.3333333333333333703, 0.3333333333333333703, 0.3333333333333333703, 0.3333333333333333703, 0.3333333333333333703, 0.3333333333333333703, 0.3333333333333333703, 0.3333333333333333703, 0.3333333333333333703, 0.3333333333333333703, 0.3333333333333333703, 0.3333333333333333703, 0.3333333333333333703, 0.3333333333333333703, 0.3333333333333333703, 0.3333333333333333703, 0.3333333333333333703, 0.3333333333333333703, 0.3333333333333333703, 0.3333333333333333703, 0.3333333333333333703, 0.3333333333333333703, 0.3333333333333333703, 0.3333333333333333703, 0.3333333333333333703, 0.3333333333333333703, 0.3333333333333333703, 0.3333333333333333703, 0.3333333333333333703, 0.3333333333333333703, 0.3333333333333333703, 0.3333333333333333703, 0.3333333333333333703, 0.3333333333333333703, 0.3333333333333333703, 0.3333333333333333703, 0.3333333333333333703, 0.3333333333333333703, 0.3333333333333333703, 0.3333333333333333703, 0.3333333333333333703, 0.3333333333333333703, 0.3333333333333333703, 0.3333333333333333703, 0.3333333333333333703, 0.3333333333333333703, 0.3333333333333333703, 0.3333333333333333703, 0.3333333333333333703, 0.3333333333333333703, 0.3333333333333333703, 0.3333333333333333703, 0.3333333333333333703, 0.3333333333333333703, 0.3333333333333333703, 0.3333333333333333703, 0.3333333333333333703, 0.3333333333333333703, 0.3333333333333333703, 0.3333333333333333703, 0.3333333333333333703, 0.3333333333333333703, 0.3333333333333333703, 0.3333333333333333703, 0.3333333333333333703),
 ( 0.3333333333333333703, 0.3333333333333333703, 0.3333333333333333703, 0.3333333333333333703, 0.3333333333333333703, 0.3333333333333333703, 0.3333333333333333703, 0.3333333333333333703, 0.3333333333333333703, 0.3333333333333333703, 0.3333333333333333703, 0.3333333333333333703, 0.3333333333333333703, 0.3333333333333333703, 0.3333333333333333703, 0.3333333333333333703, 0.3333333333333333703, 0.3333333333333333703, 0.3333333333333333703, 0.3333333333333333703, 0.3333333333333333703, 0.3333333333333333703, 0.3333333333333333703, 0.3333333333333333703, 0.3333333333333333703, 0.3333333333333333703, 0.3333333333333333703, 0.3333333333333333703, 0.3333333333333333703, 0.3333333333333333703, 0.3333333333333333703, 0.3333333333333333703, 0.3333333333333333703, 0.3333333333333333703, 0.3333333333333333703, 0.3333333333333333703, 0.3333333333333333703, 0.3333333333333333703, 0.3333333333333333703, 0.3333333333333333703, 0.3333333333333333703, 0.3333333333333333703, 0.3333333333333333703, 0.3333333333333333703, 0.3333333333333333703, 0.3333333333333333703, 0.3333333333333333703, 0.3333333333333333703, 0.3333333333333333703, 0.3333333333333333703, 0.3333333333333333703, 0.3333333333333333703, 0.3333333333333333703, 0.3333333333333333703, 0.3333333333333333703, 0.3333333333333333703, 0.3333333333333333703, 0.3333333333333333703, 0.3333333333333333703, 0.3333333333333333703, 0.3333333333333333703, 0.3333333333333333703, 0.3333333333333333703, 0.3333333333333333703, 0.3333333333333333703, 0.3333333333333333703, 0.3333333333333333703, 0.3333333333333333703, 0.3333333333333333703, 0.3333333333333333703, 0.3333333333333333703, 0.3333333333333333703, 0.3333333333333333703, 0.3333333333333333703, 0.3333333333333333703, 0.3333333333333333703, 0.3333333333333333703, 0.3333333333333333703, 0.3333333333333333703, 0.3333333333333333703, 0.3333333333333333703, 0.3333333333333333703, 0.3333333333333333703, 0.3333333333333333703, 0.3333333333333333703, 0.3333333333333333703),
 ( 1.000000000000000000, 1.000000000000000000, 1.000000000000000000, 1.000000000000000000, 1.000000000000000000, 1.000000000000000000, 1.000000000000000000, 1.000000000000000000, 1.000000000000000000, 1.000000000000000000, 1.000000000000000000, 1.000000000000000000, 1.000000000000000000, 1.000000000000000000, 1.000000000000000000, 1.000000000000000000, 1.000000000000000000, 1.000000000000000000, 1.000000000000000000, 1.000000000000000000, 1.000000000000000000, 1.000000000000000000, 1.000000000000000000, 1.000000000000000000, 1.000000000000000000, 1.000000000000000000, 1.000000000000000000, 1.000000000000000000, 1.000000000000000000, 1.000000000000000000, 1.000000000000000000, 1.000000000000000000, 1.000000000000000000, 1.000000000000000000, 1.000000000000000000, 1.000000000000000000, 1.000000000000000000, 1.000000000000000000, 1.000000000000000000, 1.000000000000000000, 1.000000000000000000, 1.000000000000000000, 1.000000000000000000, 1.000000000000000000, 1.000000000000000000, 1.000000000000000000, 1.000000000000000000, 1.000000000000000000, 1.000000000000000000, 1.000000000000000000, 1.000000000000000000, 1.000000000000000000, 1.000000000000000000, 1.000000000000000000, 1.000000000000000000, 1.000000000000000000, 1.000000000000000000, 1.000000000000000000, 1.000000000000000000, 1.000000000000000000, 1.000000000000000000, 1.000000000000000000, 1.000000000000000000, 1.000000000000000000, 1.000000000000000000, 1.000000000000000000, 1.000000000000000000, 1.000000000000000000, 1.000000000000000000, 1.000000000000000000, 1.000000000000000000, 1.000000000000000000, 1.000000000000000000, 1.000000000000000000, 1.000000000000000000, 1.000000000000000000, 1.000000000000000000, 1.000000000000000000, 1.000000000000000000, 1.000000000000000000, 1.000000000000000000, 1.000000000000000000, 1.000000000000000000, 1.000000000000000000, 1.000000000000000000, 1.000000000000000000),
 ( 0.3333333333333333703, 0.3333333333333333703, 0.3333333333333333703, 0.3333333333333333703, 0.3333333333333333703, 0.3333333333333333703, 0.3333333333333333703, 0.3333333333333333703, 0.3333333333333333703, 0.3333333333333333703, 0.3333333333333333703, 0.3333333333333333703, 0.3333333333333333703, 0.3333333333333333703, 0.3333333333333333703, 0.3333333333333333703, 0.3333333333333333703, 0.3333333333333333703, 0.3333333333333333703, 0.3333333333333333703, 0.3333333333333333703, 0.3333333333333333703, 0.3333333333333333703, 0.3333333333333333703, 0.3333333333333333703, 0.3333333333333333703, 0.3333333333333333703, 0.3333333333333333703, 0.3333333333333333703, 0.3333333333333333703, 0.3333333333333333703, 0.3333333333333333703, 0.3333333333333333703, 0.3333333333333333703, 0.3333333333333333703, 0.3333333333333333703, 0.3333333333333333703, 0.3333333333333333703, 0.3333333333333333703, 0.3333333333333333703, 0.3333333333333333703, 0.3333333333333333703, 0.3333333333333333703, 0.3333333333333333703, 0.3333333333333333703, 0.3333333333333333703, 0.3333333333333333703, 0.3333333333333333703, 0.3333333333333333703, 0.3333333333333333703, 0.3333333333333333703, 0.3333333333333333703, 0.3333333333333333703, 0.3333333333333333703, 0.3333333333333333703, 0.3333333333333333703, 0.3333333333333333703, 0.3333333333333333703, 0.3333333333333333703, 0.3333333333333333703, 0.3333333333333333703, 0.3333333333333333703, 0.3333333333333333703, 0.3333333333333333703, 0.3333333333333333703, 0.3333333333333333703, 0.3333333333333333703, 0.3333333333333333703, 0.3333333333333333703, 0.3333333333333333703, 0.3333333333333333703, 0.3333333333333333703, 0.3333333333333333703, 0.3333333333333333703, 0.3333333333333333703, 0.3333333333333333703, 0.3333333333333333703, 0.3333333333333333703, 0.3333333333333333703, 0.3333333333333333703, 0.3333333333333333703, 0.3333333333333333703, 0.3333333333333333703, 0.3333333333333333703, 0.3333333333333333703, 0.3333333333333333703),
 ( 0.3333333333333333703, 0.3333333333333333703, 0.3333333333333333703, 0.3333333333333333703, 0.3333333333333333703, 0.3333333333333333703, 0.3333333333333333703, 0.3333333333333333703, 0.3333333333333333703, 0.3333333333333333703, 0.3333333333333333703, 0.3333333333333333703, 0.3333333333333333703, 0.3333333333333333703, 0.3333333333333333703, 0.3333333333333333703, 0.3333333333333333703, 0.3333333333333333703, 0.3333333333333333703, 0.3333333333333333703, 0.3333333333333333703, 0.3333333333333333703, 0.3333333333333333703, 0.3333333333333333703, 0.3333333333333333703, 0.3333333333333333703, 0.3333333333333333703, 0.3333333333333333703, 0.3333333333333333703, 0.3333333333333333703, 0.3333333333333333703, 0.3333333333333333703, 0.3333333333333333703, 0.3333333333333333703, 0.3333333333333333703, 0.3333333333333333703, 0.3333333333333333703, 0.3333333333333333703, 0.3333333333333333703, 0.3333333333333333703, 0.3333333333333333703, 0.3333333333333333703, 0.3333333333333333703, 0.3333333333333333703, 0.3333333333333333703, 0.3333333333333333703, 0.3333333333333333703, 0.3333333333333333703, 0.3333333333333333703, 0.3333333333333333703, 0.3333333333333333703, 0.3333333333333333703, 0.3333333333333333703, 0.3333333333333333703, 0.3333333333333333703, 0.3333333333333333703, 0.3333333333333333703, 0.3333333333333333703, 0.3333333333333333703, 0.3333333333333333703, 0.3333333333333333703, 0.3333333333333333703, 0.3333333333333333703, 0.3333333333333333703, 0.3333333333333333703, 0.3333333333333333703, 0.3333333333333333703, 0.3333333333333333703, 0.3333333333333333703, 0.3333333333333333703, 0.3333333333333333703, 0.3333333333333333703, 0.3333333333333333703, 0.3333333333333333703, 0.3333333333333333703, 0.3333333333333333703, 0.3333333333333333703, 0.3333333333333333703, 0.3333333333333333703, 0.3333333333333333703, 0.3333333333333333703, 0.3333333333333333703, 0.3333333333333333703, 0.3333333333333333703, 0.3333333333333333703, 0.3333333333333333703),
 ( 1.000000000000000000, 1.000000000000000000, 1.000000000000000000, 1.000000000000000000, 1.000000000000000000, 1.000000000000000000, 1.000000000000000000, 1.000000000000000000, 1.000000000000000000, 1.000000000000000000, 1.000000000000000000, 1.000000000000000000, 1.000000000000000000, 1.000000000000000000, 1.000000000000000000, 1.000000000000000000, 1.000000000000000000, 1.000000000000000000, 1.000000000000000000, 1.000000000000000000, 1.000000000000000000, 1.000000000000000000, 1.000000000000000000, 1.000000000000000000, 1.000000000000000000, 1.000000000000000000, 1.000000000000000000, 1.000000000000000000, 1.000000000000000000, 1.000000000000000000, 1.000000000000000000, 1.000000000000000000, 1.000000000000000000, 1.000000000000000000, 1.000000000000000000, 1.000000000000000000, 1.000000000000000000, 1.000000000000000000, 1.000000000000000000, 1.000000000000000000, 1.000000000000000000, 1.000000000000000000, 1.000000000000000000, 1.000000000000000000, 1.000000000000000000, 1.000000000000000000, 1.000000000000000000, 1.000000000000000000, 1.000000000000000000, 1.000000000000000000, 1.000000000000000000, 1.000000000000000000, 1.000000000000000000, 1.000000000000000000, 1.000000000000000000, 1.000000000000000000, 1.000000000000000000, 1.000000000000000000, 1.000000000000000000, 1.000000000000000000, 1.000000000000000000, 1.000000000000000000, 1.000000000000000000, 1.000000000000000000, 1.000000000000000000, 1.000000000000000000, 1.000000000000000000, 1.000000000000000000, 1.000000000000000000, 1.000000000000000000, 1.000000000000000000, 1.000000000000000000, 1.000000000000000000, 1.000000000000000000, 1.000000000000000000, 1.000000000000000000, 1.000000000000000000, 1.000000000000000000, 1.000000000000000000, 1.000000000000000000, 1.000000000000000000, 1.000000000000000000, 1.000000000000000000, 1.000000000000000000, 1.000000000000000000, 1.000000000000000000) ) ) 
 REPRESENTATION_ITEM ( '' )  SURFACE ( )  );
#6275 = DIRECTION ( 'NONE',  ( 1.000000000000000000, -0.000000000000000000, 0.000000000000000000 ) ) ;
#6276 = CARTESIAN_POINT ( 'NONE',  ( -13.84501469867711698, 4.235742283194553259, 4.833333333333343695 ) ) ;
#6277 = CARTESIAN_POINT ( 'NONE',  ( 13.37155858231679595, -19.49999999999998934, 3.449312527122348371 ) ) ;
#6278 = CARTESIAN_POINT ( 'NONE',  ( -12.65017171054692113, -19.72882861737994631, 6.192581331858542981 ) ) ;
#6279 = EDGE_CURVE ( 'NONE', #15974, #19423, #14393, .T. ) ;
#6280 = LINE ( 'NONE', #1575, #16397 ) ;
#6281 = CARTESIAN_POINT ( 'NONE',  ( 8.590308582316794173, -21.32581373872472597, 1.729004561291657582 ) ) ;
#6282 = CARTESIAN_POINT ( 'NONE',  ( 4.753441417683176518, -21.94931252712233061, 2.499999999999999112 ) ) ;
#6283 = CARTESIAN_POINT ( 'NONE',  ( -11.12844141768317741, -20.24999999999999289, 3.550687472877664952 ) ) ;
#6284 = VECTOR ( 'NONE', #3836, 1000.000000000000000 ) ;
#6285 = ORIENTED_EDGE ( 'NONE', *, *, #6337, .F. ) ;
#6286 = EDGE_CURVE ( 'NONE', #16176, #14054, #17947, .T. ) ;
#6287 = CARTESIAN_POINT ( 'NONE',  ( 13.37505992445764136, -19.49697381488866554, 4.539006848837218833 ) ) ;
#6288 = EDGE_CURVE ( 'NONE', #5732, #12390, #6965, .T. ) ;
#6289 = DIRECTION ( 'NONE',  ( 0.000000000000000000, 0.000000000000000000, 1.000000000000000000 ) ) ;
#6290 = VECTOR ( 'NONE', #9089, 1000.000000000000000 ) ;
#6291 = ORIENTED_EDGE ( 'NONE', *, *, #7873, .T. ) ;
#6292 = ORIENTED_EDGE ( 'NONE', *, *, #17759, .F. ) ;
#6293 = LINE ( 'NONE', #128, #5099 ) ;
#6294 = DIRECTION ( 'NONE',  ( -1.000000000000000000, 0.000000000000000000, 0.000000000000000000 ) ) ;
#6295 = CIRCLE ( 'NONE', #2623, 0.2500000000000002220 ) ;
#6296 = CARTESIAN_POINT ( 'NONE',  ( -3.882031223148668886, -13.81156101447257889, 3.771450735391772557 ) ) ;
#6297 = CARTESIAN_POINT ( 'NONE',  ( 27.44203811574919882, 0.000000000000000000, 0.000000000000000000 ) ) ;
#6298 = VECTOR ( 'NONE', #4327, 1000.000000000000000 ) ;
#6299 = LINE ( 'NONE', #6199, #15050 ) ;
#6300 = CARTESIAN_POINT ( 'NONE',  ( -12.63249216759192350, -19.87164553660301536, 5.297612231341934041 ) ) ;
#6301 = CARTESIAN_POINT ( 'NONE',  ( 12.43405858231679417, -23.20159541128345992, 4.773278322869455970 ) ) ;
#6302 = FACE_OUTER_BOUND ( 'NONE', #3777, .T. ) ;
#6303 = CARTESIAN_POINT ( 'NONE',  ( 13.15498530132288479, 5.764257716805535559, 4.833333333333343695 ) ) ;
#6304 = EDGE_CURVE ( 'NONE', #10907, #6038, #16106, .T. ) ;
#6305 = CARTESIAN_POINT ( 'NONE',  ( -5.871558582316795949, -19.49999999999998934, 3.449312527122348371 ) ) ;
#6306 = CARTESIAN_POINT ( 'NONE',  ( -2.081625295426255295, -10.37614485793134556, 1.753937271548854815 ) ) ;
#6307 = ORIENTED_EDGE ( 'NONE', *, *, #15488, .F. ) ;
#6308 = CARTESIAN_POINT ( 'NONE',  ( -13.84137125862932649, 4.051748560779529384, 5.236069268230914453 ) ) ;
#6309 = CARTESIAN_POINT ( 'NONE',  ( 10.38119784648305810, -14.00000000000000000, 2.000000000000000000 ) ) ;
#6310 = CARTESIAN_POINT ( 'NONE',  ( 12.34719141768317563, -21.22443879296941915, 1.770995438708345748 ) ) ;
#6311 = CARTESIAN_POINT ( 'NONE',  ( -6.253441417683175629, -21.94931252712233061, 2.499999999999999112 ) ) ;
#6312 = VERTEX_POINT ( 'NONE', #11771 ) ;
#6313 = VECTOR ( 'NONE', #15866, 1000.000000000000000 ) ;
#6314 = CARTESIAN_POINT ( 'NONE',  ( 13.87367531042247748, 4.933103176334663331, 5.324010972534209074 ) ) ;
#6315 = CARTESIAN_POINT ( 'NONE',  ( 12.62500000000001954, -20.25000000000274269, 4.083333333315724012 ) ) ;
#6316 = VECTOR ( 'NONE', #3930, 1000.000000000000000 ) ;
#6317 = CARTESIAN_POINT ( 'NONE',  ( -9.999999999999998224, -30.00000000000000355, 0.000000000000000000 ) ) ;
#6318 = VERTEX_POINT ( 'NONE', #18373 ) ;
#6319 = VECTOR ( 'NONE', #5544, 1000.000000000000000 ) ;
#6320 = VERTEX_POINT ( 'NONE', #583 ) ;
#6321 = DIRECTION ( 'NONE',  ( 1.000000000000000000, 0.000000000000000000, -0.000000000000000000 ) ) ;
#6322 = EDGE_CURVE ( 'NONE', #13949, #6936, #7279, .T. ) ;
#6323 = CARTESIAN_POINT ( 'NONE',  ( -24.79469207716615031, 0.000000000000000000, 1.000000000000000000 ) ) ;
#6324 = LINE ( 'NONE', #8110, #624 ) ;
#6325 = PLANE ( 'NONE',  #19559 ) ;
#6326 = CARTESIAN_POINT ( 'NONE',  ( 2.659620708751979645, -10.38426118526329489, 2.698636689302993830 ) ) ;
#6327 = DIRECTION ( 'NONE',  ( 0.000000000000000000, 1.000000000000000000, -0.000000000000000000 ) ) ;
#6328 = CARTESIAN_POINT ( 'NONE',  ( 2.844469389063872811, -10.54053385813977606, 1.988770633557972012 ) ) ;
#6329 = DIRECTION ( 'NONE',  ( 0.000000000000000000, 0.000000000000000000, -1.000000000000000000 ) ) ;
#6330 = CIRCLE ( 'NONE', #9009, 0.3749999999999997224 ) ;
#6331 = DIRECTION ( 'NONE',  ( 1.000000000000000000, 0.000000000000000000, 0.000000000000000000 ) ) ;
#6332 = EDGE_CURVE ( 'NONE', #17187, #11652, #5428, .T. ) ;
#6333 = DIRECTION ( 'NONE',  ( -0.000000000000000000, -0.000000000000000000, -1.000000000000000000 ) ) ;
#6334 = AXIS2_PLACEMENT_3D ( 'NONE', #15930, #1412, #46 ) ;
#6335 = LINE ( 'NONE', #11453, #10650 ) ;
#6336 = LINE ( 'NONE', #1735, #17397 ) ;
#6337 = EDGE_CURVE ( 'NONE', #12047, #13360, #794, .T. ) ;
#6338 = CARTESIAN_POINT ( 'NONE',  ( -2.623717082130370137, -10.12934627674766830, 2.633169448359191644 ) ) ;
#6339 = PRODUCT ( 'Moving Upper Ceramic Cutting Blade', 'Moving Upper Ceramic Cutting Blade', '', ( #14733 ) ) ;
#6340 = CARTESIAN_POINT ( 'NONE',  ( 5.128441417683177406, -20.99999999999999645, 3.550687472877664952 ) ) ;
#6341 = CARTESIAN_POINT ( 'NONE',  ( -13.09892531043291086, 3.683228176858501790, 6.000681092915118420 ) ) ;
#6342 = CARTESIAN_POINT ( 'NONE',  ( -6.996558582316795949, -22.05068747287764452, 2.499999999999999112 ) ) ;
#6343 = VECTOR ( 'NONE', #16112, 1000.000000000000000 ) ;
#6344 = CARTESIAN_POINT ( 'NONE',  ( -12.44094141768317741, -20.72672167713052715, 2.298404588716546293 ) ) ;
#6345 = EDGE_CURVE ( 'NONE', #6014, #18185, #9757, .T. ) ;
#6346 = EDGE_LOOP ( 'NONE', ( #12869, #11886, #18495, #1897 ) ) ;
#6347 = CARTESIAN_POINT ( 'NONE',  ( 13.37499999999998224, -19.49999999999998934, 4.166666666666637653 ) ) ;
#6348 = LINE ( 'NONE', #17431, #5874 ) ;
#6349 = ORIENTED_EDGE ( 'NONE', *, *, #17554, .T. ) ;
#6350 = CARTESIAN_POINT ( 'NONE',  ( 20.00000000000000000, 5.204170427930421283E-15, 2.000000000000000000 ) ) ;
#6351 = ORIENTED_EDGE ( 'NONE', *, *, #1409, .T. ) ;
#6352 = DIRECTION ( 'NONE',  ( 0.000000000000000000, 0.000000000000000000, 1.000000000000000000 ) ) ;
#6353 = CIRCLE ( 'NONE', #11681, 10.00000000000000000 ) ;
#6354 = EDGE_CURVE ( 'NONE', #6936, #3922, #2056, .T. ) ;
#6355 = COLOUR_RGB ( '', 0.09019608, 0.27058824, 0.51372549) ;
#6356 = VECTOR ( 'NONE', #19393, 1000.000000000000000 ) ;
#6357 = ORIENTED_EDGE ( 'NONE', *, *, #9821, .T. ) ;
#6358 = CARTESIAN_POINT ( 'NONE',  ( 12.62672070884157804, -20.24999999999983658, 3.550922209436377042 ) ) ;
#6359 = DIRECTION ( 'NONE',  ( 0.000000000000000000, 1.000000000000000000, 0.000000000000000000 ) ) ;
#6360 = AXIS2_PLACEMENT_3D ( 'NONE', #12960, #19361, #1882 ) ;
#6361 = CARTESIAN_POINT ( 'NONE',  ( -2.731427961995660958, -10.89409100229510052, 2.829571171190552015 ) ) ;
#6362 = DIRECTION ( 'NONE',  ( 0.000000000000000000, -0.000000000000000000, 1.000000000000000000 ) ) ;
#6363 = CARTESIAN_POINT ( 'NONE',  ( -8.871558582316794173, -20.24999999999999289, 3.449312527122348371 ) ) ;
#6364 =( LENGTH_UNIT ( ) NAMED_UNIT ( * ) SI_UNIT ( .MILLI., .METRE. ) );
#6365 = CARTESIAN_POINT ( 'NONE',  ( 6.909691417683176518, -21.01515356694492098, 6.020995438708349745 ) ) ;
#6366 = DIRECTION ( 'NONE',  ( 1.000000000000000000, 0.000000000000000000, -0.000000000000000000 ) ) ;
#6367 = CARTESIAN_POINT ( 'NONE',  ( -6.159691417683176518, -22.67418626127524917, 1.729004561291651809 ) ) ;
#6368 = ORIENTED_EDGE ( 'NONE', *, *, #4649, .T. ) ;
#6369 = CARTESIAN_POINT ( 'NONE',  ( 8.590308582316794173, -21.32581373872472597, 1.729004561291657582 ) ) ;
#6370 = CARTESIAN_POINT ( 'NONE',  ( -0.000000000000000000, 11.64110105645932691, 0.000000000000000000 ) ) ;
#6371 = CARTESIAN_POINT ( 'NONE',  ( -12.62499999999998224, -20.99999999999998934, 4.166666666666637653 ) ) ;
#6372 = ORIENTED_EDGE ( 'NONE', *, *, #1139, .F. ) ;
#6373 = VECTOR ( 'NONE', #1223, 1000.000000000000000 ) ;
#6374 = AXIS2_PLACEMENT_3D ( 'NONE', #4464, #2682, #9266 ) ;
#6375 = CARTESIAN_POINT ( 'NONE',  ( 7.840308582316794173, -22.67418626127525982, 5.270995438708342640 ) ) ;
#6376 = PLANE ( 'NONE',  #7665 ) ;
#6377 = VECTOR ( 'NONE', #20046, 1000.000000000000000 ) ;
#6378 = EDGE_LOOP ( 'NONE', ( #16151, #12002, #12511, #4448 ) ) ;
#6379 = CARTESIAN_POINT ( 'NONE',  ( 0.000000000000000000, 10.00000000000000000, 1.000000000000000000 ) ) ;
#6380 =( LENGTH_UNIT ( ) NAMED_UNIT ( * ) SI_UNIT ( .MILLI., .METRE. ) );
#6381 = ORIENTED_EDGE ( 'NONE', *, *, #13316, .T. ) ;
#6382 = EDGE_CURVE ( 'NONE', #16371, #9021, #3617, .T. ) ;
#6383 = CARTESIAN_POINT ( 'NONE',  ( 3.469446951953523943E-14, 10.00000000000009592, 0.000000000000000000 ) ) ;
#6384 = EDGE_LOOP ( 'NONE', ( #11659, #10901, #2450, #8096 ) ) ;
#6385 = CARTESIAN_POINT ( 'NONE',  ( -7.184058582316794173, -20.79840458871652942, 2.226721677130544030 ) ) ;
#6386 = DIRECTION ( 'NONE',  ( 0.000000000000000000, 0.000000000000000000, 1.000000000000000000 ) ) ;
#6387 = DIRECTION ( 'NONE',  ( 0.000000000000000000, 0.2588190451025245697, 0.9659258262890673130 ) ) ;
#6388 = CARTESIAN_POINT ( 'NONE',  ( 2.167793999318431197, -10.98794063836983703, 1.911058649813994315 ) ) ;
#6389 = VECTOR ( 'NONE', #6230, 1000.000000000000000 ) ;
#6390 = VECTOR ( 'NONE', #3049, 1000.000000000000000 ) ;
#6391 = DIRECTION ( 'NONE',  ( -4.625929269271486111E-15, -1.000000000000000000, 0.000000000000000000 ) ) ;
#6392 = CARTESIAN_POINT ( 'NONE',  ( -13.84256985046264710, 4.112277448363203192, 5.213861325540929847 ) ) ;
#6394 = CARTESIAN_POINT ( 'NONE',  ( 6.527808582316794173, -23.72900456129165647, 4.275561207030568411 ) ) ;
#6393 = VECTOR ( 'NONE', #14887, 1000.000000000000000 ) ;
#6395 = CARTESIAN_POINT ( 'NONE',  ( -13.90439706815434739, 5.734551941788608609, 5.045486763335835789 ) ) ;
#6396 = PLANE ( 'NONE',  #6731 ) ;
#6397 = CARTESIAN_POINT ( 'NONE',  ( -5.215308582316795949, -24.52099543870834708, 2.515153566944913432 ) ) ;
#6398 = CARTESIAN_POINT ( 'NONE',  ( 5.496558582316794173, -22.05068747287764452, 1.749999999999998446 ) ) ;
#6399 = CARTESIAN_POINT ( 'NONE',  ( 7.565941417683177406, -22.67126532539353789, 2.757051763020445634 ) ) ;
#6400 = CARTESIAN_POINT ( 'NONE',  ( -8.690941417683177406, -23.27327832286946219, 4.701595411283453707 ) ) ;
#6401 = ORIENTED_EDGE ( 'NONE', *, *, #20235, .F. ) ;
#6402 = CARTESIAN_POINT ( 'NONE',  ( 13.83890698502169059, 3.927302743594121903, 5.241364546715693074 ) ) ;
#6403 = CIRCLE ( 'NONE', #4599, 1.000000000000002665 ) ;
#6404 = CARTESIAN_POINT ( 'NONE',  ( -2.693754455098655409, -10.04853567022903782, 2.237415670251142519 ) ) ;
#6405 = ORIENTED_EDGE ( 'NONE', *, *, #8813, .T. ) ;
#6406 = VECTOR ( 'NONE', #12066, 1000.000000000000000 ) ;
#6407 = ORIENTED_EDGE ( 'NONE', *, *, #20532, .F. ) ;
#6408 = CARTESIAN_POINT ( 'NONE',  ( 29.18266749954691619, 14.63532295040229059, 0.3390567389149258815 ) ) ;
#6409 = CARTESIAN_POINT ( 'NONE',  ( -12.00000000000000000, -25.49999999999998934, 4.000000000000000000 ) ) ;
#6410 = EDGE_CURVE ( 'NONE', #11562, #15034, #10207, .T. ) ;
#6411 = CARTESIAN_POINT ( 'NONE',  ( 13.49999999999998401, -24.47992105705875332, 12.00000000000000000 ) ) ;
#6412 = CARTESIAN_POINT ( 'NONE',  ( -3.379380450443691952, -10.24275229525297348, 2.854909362179569587 ) ) ;
#6413 = FACE_OUTER_BOUND ( 'NONE', #9055, .T. ) ;
#6414 = EDGE_CURVE ( 'NONE', #8228, #1847, #1561, .T. ) ;
#6415 = CARTESIAN_POINT ( 'NONE',  ( 2.309828811027716977, -9.292785183284841821, 1.668323847571005603 ) ) ;
#6416 = CARTESIAN_POINT ( 'NONE',  ( -13.10372118337080849, 3.925419760224517329, 6.005889426248455010 ) ) ;
#6417 = CARTESIAN_POINT ( 'NONE',  ( 13.18405858231679417, -20.79840458871652942, 2.226721677130544030 ) ) ;
#6418 = EDGE_CURVE ( 'NONE', #4642, #15518, #18677, .T. ) ;
#6419 = DIRECTION ( 'NONE',  ( -0.000000000000000000, -0.000000000000000000, -1.000000000000000000 ) ) ;
#6420 = CARTESIAN_POINT ( 'NONE',  ( 13.11465082267961968, 3.727366545318180791, 6.751662912489328150 ) ) ;
#6421 = VECTOR ( 'NONE', #7528, 1000.000000000000000 ) ;
#6422 = CARTESIAN_POINT ( 'NONE',  ( -1.857501949683560971, -9.975525523312803955, 2.401050223243493154 ) ) ;
#6423 = ORIENTED_EDGE ( 'NONE', *, *, #11065, .T. ) ;
#6424 = CARTESIAN_POINT ( 'NONE',  ( -13.85163507668220539, 3.820071372449974412, 5.989091157956555556 ) ) ;
#6425 = LINE ( 'NONE', #8099, #20087 ) ;
#6426 = CARTESIAN_POINT ( 'NONE',  ( 8.315941417683177406, -20.26807450282663225, 5.303608408759377113 ) ) ;
#6427 = CARTESIAN_POINT ( 'NONE',  ( -12.05905858231679595, -21.25705176302045274, 4.171265325393551215 ) ) ;
#6428 = ORIENTED_EDGE ( 'NONE', *, *, #14082, .F. ) ;
#6429 = CARTESIAN_POINT ( 'NONE',  ( 13.90439735423812273, 5.734566389025032684, 3.666666666666500873 ) ) ;
#6430 = CARTESIAN_POINT ( 'NONE',  ( 12.66369984131459070, -18.29565801360988075, 5.528024842915327142 ) ) ;
#6431 = CYLINDRICAL_SURFACE ( 'NONE', #18707, 10.00000000000000000 ) ;
#6432 = ORIENTED_EDGE ( 'NONE', *, *, #8864, .F. ) ;
#6433 = EDGE_LOOP ( 'NONE', ( #19141, #15004, #18087, #17264, #12137, #17651 ) ) ;
#6434 = CARTESIAN_POINT ( 'NONE',  ( -1.734723475976795735E-14, 10.00000000000004619, 1.000000000000000000 ) ) ;
#6435 = VECTOR ( 'NONE', #11567, 1000.000000000000000 ) ;
#6436 = ADVANCED_FACE ( 'NONE', ( #20353 ), #13950, .T. ) ;
#6437 = CARTESIAN_POINT ( 'NONE',  ( 0.000000000000000000, 9.000000000000001776, 1.000000000000000000 ) ) ;
#6438 = CARTESIAN_POINT ( 'NONE',  ( 20.00000000000000000, 3.500000000000004885, 1.000000000000000000 ) ) ;
#6439 = CARTESIAN_POINT ( 'NONE',  ( -2.601332995093193379, -9.970398767539743190, 2.592349323443654097 ) ) ;
#6440 = EDGE_CURVE ( 'NONE', #7250, #8074, #2982, .T. ) ;
#6441 = CARTESIAN_POINT ( 'NONE',  ( 0.000000000000000000, 11.64110105645932691, 10.00000000000000000 ) ) ;
#6442 = CARTESIAN_POINT ( 'NONE',  ( 2.022757268986824730, -10.07035769906783784, 1.675405020440470238 ) ) ;
#6443 = CARTESIAN_POINT ( 'NONE',  ( -25.29469207716615031, 9.000000000000001776, 0.000000000000000000 ) ) ;
#6444 = EDGE_CURVE ( 'NONE', #13250, #14757, #17612, .T. ) ;
#6445 = CARTESIAN_POINT ( 'NONE',  ( 3.499999999999999556, -24.49999999999999289, 4.000000000000000000 ) ) ;
#6446 = CARTESIAN_POINT ( 'NONE',  ( 21.17243175760212637, 9.000000000000001776, 1.000000000000000000 ) ) ;
#6447 = DIRECTION ( 'NONE',  ( 0.000000000000000000, -0.9919684228235026158, -0.1264857625231113336 ) ) ;
#6448 = CARTESIAN_POINT ( 'NONE',  ( -11.30905858231679417, -23.27327832286945153, 2.298404588716537411 ) ) ;
#6449 = CARTESIAN_POINT ( 'NONE',  ( -2.659620708751979645, -10.38426118526329489, 2.698636689302993830 ) ) ;
#6450 = CARTESIAN_POINT ( 'NONE',  ( 11.68405858231679595, -21.32873467460644079, 2.757051763020455404 ) ) ;
#6451 = CARTESIAN_POINT ( 'NONE',  ( -13.08919463935856697, 3.941829287606363863, 5.256209690007596080 ) ) ;
#6452 = CARTESIAN_POINT ( 'NONE',  ( -7.184058582316795949, -21.32873467460644079, 2.757051763020455404 ) ) ;
#6453 = AXIS2_PLACEMENT_3D ( 'NONE', #5787, #18547, #1284 ) ;
#6454 = CARTESIAN_POINT ( 'NONE',  ( -10.37844141768317741, -23.74999999999999645, 3.449312527122335492 ) ) ;
#6455 = ORIENTED_EDGE ( 'NONE', *, *, #227, .T. ) ;
#6456 = CARTESIAN_POINT ( 'NONE',  ( 13.09173631808601002, 4.070184063342107805, 5.250510817581989009 ) ) ;
#6457 = PRESENTATION_STYLE_ASSIGNMENT (( #70 ) ) ;
#6458 = ORIENTED_EDGE ( 'NONE', *, *, #10516, .T. ) ;
#6459 = ORIENTED_EDGE ( 'NONE', *, *, #9109, .F. ) ;
#6460 = DIRECTION ( 'NONE',  ( -0.000000000000000000, 0.000000000000000000, 1.000000000000000000 ) ) ;
#6461 = CARTESIAN_POINT ( 'NONE',  ( 13.41115317570721110, -19.17426462678482579, 6.244630269197427808 ) ) ;
#6462 = VERTEX_POINT ( 'NONE', #15834 ) ;
#6463 = CARTESIAN_POINT ( 'NONE',  ( 20.00000000000000000, 3.500000000000004885, 1.500000000000000000 ) ) ;
#6464 = ADVANCED_FACE ( 'NONE', ( #9463 ), #14160, .F. ) ;
#6465 = AXIS2_PLACEMENT_3D ( 'NONE', #15151, #18095, #18193 ) ;
#6466 = EDGE_CURVE ( 'NONE', #16994, #10660, #16050, .T. ) ;
#6467 = ORIENTED_EDGE ( 'NONE', *, *, #795, .F. ) ;
#6468 = CARTESIAN_POINT ( 'NONE',  ( 10.00344141768317563, -22.05068747287765873, 5.250000000000000888 ) ) ;
#6469 = AXIS2_PLACEMENT_3D ( 'NONE', #332, #1160, #2613 ) ;
#6470 = DIRECTION ( 'NONE',  ( 0.000000000000000000, 1.000000000000000000, 0.000000000000000000 ) ) ;
#6471 = CARTESIAN_POINT ( 'NONE',  ( -2.367358971471363649, -9.400572650371021410, 2.446005822389718087 ) ) ;
#6472 = CARTESIAN_POINT ( 'NONE',  ( 2.645259258103298983, -10.28229522185712241, 2.672449792925449596 ) ) ;
#6473 = DIRECTION ( 'NONE',  ( 1.000000000000000000, 6.938893903907222067E-15, 0.000000000000000000 ) ) ;
#6474 = LINE ( 'NONE', #8341, #8636 ) ;
#6475 = CARTESIAN_POINT ( 'NONE',  ( 6.534691417683176518, -20.22900456129164581, 2.825813738724747726 ) ) ;
#6476 = CARTESIAN_POINT ( 'NONE',  ( -5.597191417683179182, -22.77556120703057729, 5.229004561291655584 ) ) ;
#6477 = ORIENTED_EDGE ( 'NONE', *, *, #3593, .F. ) ;
#6478 = CARTESIAN_POINT ( 'NONE',  ( 9.621558582316794173, -23.74999999999999645, 3.550687472877651629 ) ) ;
#6479 = CARTESIAN_POINT ( 'NONE',  ( -30.00000000000000000, 3.000000000000000000, 1.000000000000000000 ) ) ;
#6480 = CARTESIAN_POINT ( 'NONE',  ( -12.65017171054692113, -19.72882861737994631, 6.192581331858542981 ) ) ;
#6481 = ORIENTED_EDGE ( 'NONE', *, *, #14119, .F. ) ;
#6482 = CARTESIAN_POINT ( 'NONE',  ( 5.496558582316794173, -22.05068747287764452, 1.749999999999998446 ) ) ;
#6483 = LINE ( 'NONE', #19347, #6995 ) ;
#6484 = ORIENTED_EDGE ( 'NONE', *, *, #330, .T. ) ;
#6485 = CYLINDRICAL_SURFACE ( 'NONE', #20309, 0.3749999999999997224 ) ;
#6486 = ORIENTED_EDGE ( 'NONE', *, *, #1439, .T. ) ;
#6487 = ADVANCED_FACE ( 'NONE', ( #16254 ), #20662, .T. ) ;
#6488 = FACE_OUTER_BOUND ( 'NONE', #7559, .T. ) ;
#6489 = EDGE_CURVE ( 'NONE', #15669, #15962, #4644, .T. ) ;
#6490 = EDGE_LOOP ( 'NONE', ( #16835, #19655, #20339, #5339 ) ) ;
#6491 = CARTESIAN_POINT ( 'NONE',  ( -7.746558582316794173, -21.94931252712234482, 5.250000000000000888 ) ) ;
#6492 = CARTESIAN_POINT ( 'NONE',  ( 12.62500016093973620, -20.24999187254239175, 4.532396751752561848 ) ) ;
#6493 = DIRECTION ( 'NONE',  ( 0.000000000000000000, 0.000000000000000000, 1.000000000000000000 ) ) ;
#6494 = CARTESIAN_POINT ( 'NONE',  ( 2.196516900615978152, -11.19187256518208784, 1.963432442569047698 ) ) ;
#6495 = CARTESIAN_POINT ( 'NONE',  ( 12.63465172146706728, -19.76258806590802664, 5.372658420469845986 ) ) ;
#6496 = PLANE ( 'NONE',  #8359 ) ;
#6497 = CARTESIAN_POINT ( 'NONE',  ( -13.80173896975277437, 2.050317972508536535, 5.200999963382010094 ) ) ;
#6498 = CARTESIAN_POINT ( 'NONE',  ( 5.590308582316794173, -21.32581373872472597, 1.729004561291657582 ) ) ;
#6499 = CARTESIAN_POINT ( 'NONE',  ( -13.90394305879618386, 5.711624469205903942, 5.287712306078340418 ) ) ;
#6500 = EDGE_CURVE ( 'NONE', #10101, #2830, #246, .T. ) ;
#6501 = DIRECTION ( 'NONE',  ( 1.156482317317871133E-15, 1.000000000000000000, 0.000000000000000000 ) ) ;
#6502 = CARTESIAN_POINT ( 'NONE',  ( -10.65280858231679595, -20.91377862118960351, 5.979004561291660913 ) ) ;
#6503 = CARTESIAN_POINT ( 'NONE',  ( 4.746558582316793284, -21.94931252712234482, 5.250000000000000888 ) ) ;
#6504 = CARTESIAN_POINT ( 'NONE',  ( 13.18405858231679595, -21.32873467460644079, 2.757051763020455404 ) ) ;
#6505 = CARTESIAN_POINT ( 'NONE',  ( -8.972191417683177406, -23.72900456129164937, 2.724438792969417378 ) ) ;
#6506 = VERTEX_POINT ( 'NONE', #1612 ) ;
#6507 = VERTEX_POINT ( 'NONE', #12695 ) ;
#6508 = CARTESIAN_POINT ( 'NONE',  ( 13.84501469867711698, 4.235742283194553259, 4.333333333333380999 ) ) ;
#6509 = CARTESIAN_POINT ( 'NONE',  ( -0.000000000000000000, 10.00000000000000000, 0.000000000000000000 ) ) ;
#6510 = DIRECTION ( 'NONE',  ( 0.000000000000000000, 0.2487476929738665354, 0.9685683172808094987 ) ) ;
#6511 = ORIENTED_EDGE ( 'NONE', *, *, #13005, .T. ) ;
#6512 = ORIENTED_EDGE ( 'NONE', *, *, #13469, .T. ) ;
#6513 = CARTESIAN_POINT ( 'NONE',  ( -14.49999999999998579, -21.99999999999999645, 11.00000000000000178 ) ) ;
#6514 = CARTESIAN_POINT ( 'NONE',  ( -15.00000000000000000, 3.000000000000000000, 2.000000000000000000 ) ) ;
#6515 = CARTESIAN_POINT ( 'NONE',  ( 0.000000000000000000, 9.000000000000001776, 1.000000000000000000 ) ) ;
#6516 = CARTESIAN_POINT ( 'NONE',  ( -3.767139617958116471, -12.99583330722436791, 3.561955564372631500 ) ) ;
#6517 = CARTESIAN_POINT ( 'NONE',  ( -7.626396343307448866, 0.000000000000000000, 1.000000000000000000 ) ) ;
#6518 = DIRECTION ( 'NONE',  ( 1.000000000000000000, 1.156482317317871971E-16, 0.000000000000000000 ) ) ;
#6519 = CARTESIAN_POINT ( 'NONE',  ( -12.65410809543883985, -18.78004118034163739, 5.517608176248461227 ) ) ;
#6520 = FACE_OUTER_BOUND ( 'NONE', #11253, .T. ) ;
#6521 = CARTESIAN_POINT ( 'NONE',  ( -5.000000000000000000, -12.50000000000000000, 4.500000000000000888 ) ) ;
#6522 = CARTESIAN_POINT ( 'NONE',  ( 13.15498566372047762, 5.764276017890828108, 4.942557026581394730 ) ) ;
#6523 = CARTESIAN_POINT ( 'NONE',  ( -1.791727654783324741, -9.894249715907907472, 2.380176972254574697 ) ) ;
#6524 = ORIENTED_EDGE ( 'NONE', *, *, #15761, .F. ) ;
#6525 = CARTESIAN_POINT ( 'NONE',  ( -13.58606361274418184, -9.591287556442823714, 5.700679699621803209 ) ) ;
#6526 = CARTESIAN_POINT ( 'NONE',  ( 30.80549002841696904, 5.431839045955454637, 0.000000000000000000 ) ) ;
#6527 = EDGE_CURVE ( 'NONE', #5550, #3823, #6635, .T. ) ;
#6528 = AXIS2_PLACEMENT_3D ( 'NONE', #4963, #9778, #11145 ) ;
#6529 = CARTESIAN_POINT ( 'NONE',  ( 8.972191417683177406, -24.47900456129165292, 2.413778621189595963 ) ) ;
#6530 = CARTESIAN_POINT ( 'NONE',  ( -6.340308582316796837, -22.36352608949544418, 4.520995438708343528 ) ) ;
#6531 = ORIENTED_EDGE ( 'NONE', *, *, #15314, .T. ) ;
#6532 = CARTESIAN_POINT ( 'NONE',  ( 12.62672826945118665, -20.91272239271162903, 5.058631648758789900 ) ) ;
#6533 = CARTESIAN_POINT ( 'NONE',  ( 13.11514659413808737, 4.502403003978772134, 5.887634658581065494 ) ) ;
#6534 = DIRECTION ( 'NONE',  ( 0.000000000000000000, -0.000000000000000000, 1.000000000000000000 ) ) ;
#6535 = ORIENTED_EDGE ( 'NONE', *, *, #5016, .F. ) ;
#6536 = ORIENTED_EDGE ( 'NONE', *, *, #17673, .T. ) ;
#6537 = DIRECTION ( 'NONE',  ( -0.000000000000000000, -0.000000000000000000, -1.000000000000000000 ) ) ;
#6538 = FACE_OUTER_BOUND ( 'NONE', #20518, .T. ) ;
#6539 = ORIENTED_EDGE ( 'NONE', *, *, #18899, .T. ) ;
#6540 = DIRECTION ( 'NONE',  ( -1.000000000000000000, -1.734723475976809067E-16, 0.000000000000000000 ) ) ;
#6541 = CARTESIAN_POINT ( 'NONE',  ( 1.903957340438703572, -10.27085516675799148, 2.476896775482616331 ) ) ;
#6542 = LINE ( 'NONE', #6642, #11846 ) ;
#6543 = CARTESIAN_POINT ( 'NONE',  ( -27.00000000000000000, 3.000000000000000000, 1.000000000000000000 ) ) ;
#6544 = CARTESIAN_POINT ( 'NONE',  ( 5.999999999999999112, -2.500000000000047518, 2.000000000000000000 ) ) ;
#6545 = LINE ( 'NONE', #15845, #7650 ) ;
#6546 = CARTESIAN_POINT ( 'NONE',  ( 0.000000000000000000, 4.999999999999999112, 0.000000000000000000 ) ) ;
#6547 = CARTESIAN_POINT ( 'NONE',  ( -13.37500000115922383, -20.34836590895906383, 3.448843053848043017 ) ) ;
#6548 = CARTESIAN_POINT ( 'NONE',  ( -13.09358652029869141, 4.163619275088517035, 5.207983256689002083 ) ) ;
#6549 = CARTESIAN_POINT ( 'NONE',  ( -10.74655858231679417, -21.94931252712234482, 5.250000000000000888 ) ) ;
#6550 = ADVANCED_FACE ( 'NONE', ( #17826 ), #1512, .F. ) ;
#6551 = CARTESIAN_POINT ( 'NONE',  ( -5.690941417683176518, -23.27327832286946219, 4.701595411283453707 ) ) ;
#6552 = ORIENTED_EDGE ( 'NONE', *, *, #7078, .F. ) ;
#6553 = CARTESIAN_POINT ( 'NONE',  ( 13.37939227869017600, -19.27818992614120575, 4.741950614318236390 ) ) ;
#6554 = LINE ( 'NONE', #13331, #22 ) ;
#6555 = VERTEX_POINT ( 'NONE', #19097 ) ;
#6556 = EDGE_LOOP ( 'NONE', ( #17533, #11540, #11816, #9868 ) ) ;
#6557 = DIRECTION ( 'NONE',  ( 1.000000000000000000, 0.000000000000000000, 0.000000000000000000 ) ) ;
#6558 = ORIENTED_EDGE ( 'NONE', *, *, #19357, .T. ) ;
#6559 = CARTESIAN_POINT ( 'NONE',  ( 10.49999999999999645, -9.999999999999991118, 1.000000000000000000 ) ) ;
#6560 = EDGE_CURVE ( 'NONE', #17662, #11889, #6219, .T. ) ;
#6561 = EDGE_CURVE ( 'NONE', #7456, #20271, #12588, .T. ) ;
#6562 = VERTEX_POINT ( 'NONE', #1724 ) ;
#6563 = CARTESIAN_POINT ( 'NONE',  ( 11.69094141768317563, -23.27327832286946219, 4.701595411283453707 ) ) ;
#6564 = DIRECTION ( 'NONE',  ( 0.000000000000000000, 0.000000000000000000, 1.000000000000000000 ) ) ;
#6565 = CARTESIAN_POINT ( 'NONE',  ( -1.824488249492779879, -9.124319963227819130, 2.375058613629473570 ) ) ;
#6566 = CARTESIAN_POINT ( 'NONE',  ( 2.567175533087980188, -9.771398394011347577, 2.541241281345096859 ) ) ;
#6567 = CARTESIAN_POINT ( 'NONE',  ( -10.18405858231679417, -20.79840458871652942, 2.226721677130544030 ) ) ;
#6568 = CARTESIAN_POINT ( 'NONE',  ( 11.97219141768317563, -23.72900456129165292, 2.724438792969417822 ) ) ;
#6569 = DIRECTION ( 'NONE',  ( -1.000000000000000000, -0.000000000000000000, -0.000000000000000000 ) ) ;
#6570 = CARTESIAN_POINT ( 'NONE',  ( -11.69094141768317741, -22.74294823697955081, 4.171265325393542334 ) ) ;
#6571 = EDGE_CURVE ( 'NONE', #19819, #17249, #3393, .T. ) ;
#6572 = VERTEX_POINT ( 'NONE', #15933 ) ;
#6573 = CARTESIAN_POINT ( 'NONE',  ( 11.49655858231679595, -22.05068747287764452, 0.9999999999999978906 ) ) ;
#6574 = CARTESIAN_POINT ( 'NONE',  ( 12.64751377014909828, -19.11305460747000495, 5.510446717915143289 ) ) ;
#6575 = CARTESIAN_POINT ( 'NONE',  ( -12.64131715375063258, -19.42598373559290792, 5.491151580003103660 ) ) ;
#6576 = ORIENTED_EDGE ( 'NONE', *, *, #11934, .F. ) ;
#6577 = VECTOR ( 'NONE', #463, 1000.000000000000000 ) ;
#6578 = CARTESIAN_POINT ( 'NONE',  ( 0.000000000000000000, 11.64110105645932691, 10.00000000000000000 ) ) ;
#6579 = CARTESIAN_POINT ( 'NONE',  ( 21.17243175760212637, 4.999999999999999112, 0.000000000000000000 ) ) ;
#6580 = ORIENTED_EDGE ( 'NONE', *, *, #13085, .T. ) ;
#6581 = DIRECTION ( 'NONE',  ( 0.000000000000000000, 0.000000000000000000, 1.000000000000000000 ) ) ;
#6582 = ORIENTED_EDGE ( 'NONE', *, *, #17294, .F. ) ;
#6583 = DIRECTION ( 'NONE',  ( 0.000000000000000000, 0.000000000000000000, -1.000000000000000000 ) ) ;
#6584 = VECTOR ( 'NONE', #13901, 1000.000000000000000 ) ;
#6585 = ORIENTED_EDGE ( 'NONE', *, *, #6561, .T. ) ;
#6586 = EDGE_CURVE ( 'NONE', #11965, #15974, #5067, .T. ) ;
#6587 = CARTESIAN_POINT ( 'NONE',  ( -4.717959273841178636, -21.72818306014730183, 5.243595146365860771 ) ) ;
#6588 = CARTESIAN_POINT ( 'NONE',  ( 18.44064177244175440, 0.000000000000000000, 0.000000000000000000 ) ) ;
#6589 = DIRECTION ( 'NONE',  ( -0.000000000000000000, -0.000000000000000000, -1.000000000000000000 ) ) ;
#6590 = CARTESIAN_POINT ( 'NONE',  ( 1.709849555000590104, -9.864920124259167977, 1.622644547201689713 ) ) ;
#6591 = CARTESIAN_POINT ( 'NONE',  ( 13.15498530132288479, 5.764257716805535559, 4.833333333333343695 ) ) ;
#6592 = CARTESIAN_POINT ( 'NONE',  ( 4.509702210102194186, -21.62229224690691609, 4.864344626361499557 ) ) ;
#6593 = CARTESIAN_POINT ( 'NONE',  ( -13.84137125862932649, 4.051748560779529384, 5.236069268230914453 ) ) ;
#6594 = CARTESIAN_POINT ( 'NONE',  ( 8.590308582316797725, -21.01515356694490322, 0.9790045612916562501 ) ) ;
#6595 = CARTESIAN_POINT ( 'NONE',  ( -13.12860732321105139, 4.432169822159808703, 6.709107302035562270 ) ) ;
#6596 = EDGE_CURVE ( 'NONE', #12186, #3742, #8108, .T. ) ;
#6597 = EDGE_CURVE ( 'NONE', #7526, #7096, #13008, .T. ) ;
#6598 = CARTESIAN_POINT ( 'NONE',  ( 14.49999999999998579, -21.99999999999999645, 11.00000000000000178 ) ) ;
#6599 = CARTESIAN_POINT ( 'NONE',  ( 7.934058582316792396, -23.20159541128345992, 4.773278322869455970 ) ) ;
#6600 = CARTESIAN_POINT ( 'NONE',  ( 4.003441417683175629, -22.05068747287766229, 4.499999999999999112 ) ) ;
#6601 = CARTESIAN_POINT ( 'NONE',  ( -6.534691417683176518, -20.22900456129164581, 2.825813738724748170 ) ) ;
#6602 = ORIENTED_EDGE ( 'NONE', *, *, #18102, .F. ) ;
#6603 = ORIENTED_EDGE ( 'NONE', *, *, #5995, .T. ) ;
#6604 = CARTESIAN_POINT ( 'NONE',  ( 13.84501469867711698, 4.235742283194553259, 4.833333333333343695 ) ) ;
#6605 = LINE ( 'NONE', #6509, #14431 ) ;
#6606 = FILL_AREA_STYLE_COLOUR ( '', #1675 ) ;
#6607 = ORIENTED_EDGE ( 'NONE', *, *, #10917, .T. ) ;
#6608 = ORIENTED_EDGE ( 'NONE', *, *, #2725, .F. ) ;
#6609 = DIRECTION ( 'NONE',  ( 1.000000000000000000, 0.000000000000000000, -0.000000000000000000 ) ) ;
#6610 = CARTESIAN_POINT ( 'NONE',  ( -22.85856191738413656, 4.999999999999999112, 0.000000000000000000 ) ) ;
#6611 = ADVANCED_FACE ( 'NONE', ( #14364 ), #50, .T. ) ;
#6612 = DIRECTION ( 'NONE',  ( 0.000000000000000000, 1.000000000000000000, -0.000000000000000000 ) ) ;
#6613 = CARTESIAN_POINT ( 'NONE',  ( -0.2815691515810352374, -8.364917468222230923, 1.622643865078524428 ) ) ;
#6614 = CARTESIAN_POINT ( 'NONE',  ( 1.619022621591187150, -9.114917468222230923, 2.372643865078341019 ) ) ;
#6615 = CARTESIAN_POINT ( 'NONE',  ( 6.813547257480585095, 11.64110105645932691, 10.00000000000000000 ) ) ;
#6616 = CARTESIAN_POINT ( 'NONE',  ( -12.63819864697926754, -19.58346832754827105, 5.450273968536036406 ) ) ;
#6617 = CARTESIAN_POINT ( 'NONE',  ( 5.871558582316794173, -20.24999999999999289, 3.449312527122348371 ) ) ;
#6618 = VECTOR ( 'NONE', #2485, 1000.000000000000000 ) ;
#6619 = LINE ( 'NONE', #16441, #6735 ) ;
#6620 = CARTESIAN_POINT ( 'NONE',  ( 13.11145189917479392, 4.315820908324673688, 5.961432613039677086 ) ) ;
#6621 = CIRCLE ( 'NONE', #7293, 10.00000000000000000 ) ;
#6622 = CARTESIAN_POINT ( 'NONE',  ( 0.000000000000000000, -9.114917468222230923, 2.372643865078340575 ) ) ;
#6623 = ORIENTED_EDGE ( 'NONE', *, *, #16997, .F. ) ;
#6624 = CARTESIAN_POINT ( 'NONE',  ( -13.80667376788930056, 1.549525278393783179, 5.940263032956496048 ) ) ;
#6625 = CARTESIAN_POINT ( 'NONE',  ( 11.99999999999999822, -17.50000000000000000, 1.000000000000000000 ) ) ;
#6626 = VECTOR ( 'NONE', #18932, 1000.000000000000000 ) ;
#6627 = CARTESIAN_POINT ( 'NONE',  ( 7.753441417683177406, -21.94931252712233061, 0.9999999999999978906 ) ) ;
#6628 = CARTESIAN_POINT ( 'NONE',  ( -5.590308582316795949, -21.63647391050454871, 2.479004561291657804 ) ) ;
#6629 = ORIENTED_EDGE ( 'NONE', *, *, #20205, .F. ) ;
#6630 = CARTESIAN_POINT ( 'NONE',  ( 13.90439735423812273, 5.734566389025032684, 4.791666666666684726 ) ) ;
#6631 = CARTESIAN_POINT ( 'NONE',  ( 13.08573665985359824, 3.017201322601628100, 5.986358176248492313 ) ) ;
#6632 = CARTESIAN_POINT ( 'NONE',  ( 14.49999999999998579, -21.99999999999999645, 9.999999999999998224 ) ) ;
#6633 = ORIENTED_EDGE ( 'NONE', *, *, #16068, .F. ) ;
#6634 = ORIENTED_EDGE ( 'NONE', *, *, #4800, .T. ) ;
#6635 = LINE ( 'NONE', #8208, #15094 ) ;
#6636 = EDGE_CURVE ( 'NONE', #15034, #9899, #11234, .T. ) ;
#6637 = FACE_OUTER_BOUND ( 'NONE', #12481, .T. ) ;
#6638 = VECTOR ( 'NONE', #3982, 1000.000000000000000 ) ;
#6639 = VECTOR ( 'NONE', #15561, 1000.000000000000000 ) ;
#6640 = CARTESIAN_POINT ( 'NONE',  ( -14.49999999999999645, -21.00000000000000355, 4.000000000000000000 ) ) ;
#6641 = CARTESIAN_POINT ( 'NONE',  ( 1.126276606324276619, -9.864917468222230923, 1.622643865078341907 ) ) ;
#6642 = CARTESIAN_POINT ( 'NONE',  ( 10.93924542913430820, 0.000000000000000000, 1.000000000000000000 ) ) ;
#6643 = DIRECTION ( 'NONE',  ( 0.000000000000000000, 0.000000000000000000, 1.000000000000000000 ) ) ;
#6644 = FACE_OUTER_BOUND ( 'NONE', #17413, .T. ) ;
#6645 = CYLINDRICAL_SURFACE ( 'NONE', #14306, 0.5000000000000000000 ) ;
#6646 = LINE ( 'NONE', #6546, #6718 ) ;
#6647 = CARTESIAN_POINT ( 'NONE',  ( -1.957016269584227031, -9.152392576945766578, 2.382268221639079364 ) ) ;
#6648 = VECTOR ( 'NONE', #16865, 1000.000000000000000 ) ;
#6649 = VERTEX_POINT ( 'NONE', #2329 ) ;
#6650 = VECTOR ( 'NONE', #2060, 1000.000000000000000 ) ;
#6651 = CARTESIAN_POINT ( 'NONE',  ( -12.63958155142659834, -18.76363165295958524, 4.767928440007602298 ) ) ;
#6652 = CARTESIAN_POINT ( 'NONE',  ( -5.871558582316795949, -20.99999999999999645, 3.449312527122348371 ) ) ;
#6653 = CARTESIAN_POINT ( 'NONE',  ( -6.347191417683176518, -21.22443879296941915, 1.770995438708345748 ) ) ;
#6654 = VECTOR ( 'NONE', #2139, 1000.000000000000000 ) ;
#6655 = ORIENTED_EDGE ( 'NONE', *, *, #7735, .F. ) ;
#6656 = CARTESIAN_POINT ( 'NONE',  ( 13.84137125862932649, 4.051748560779529384, 5.236069268230914453 ) ) ;
#6657 = VERTEX_POINT ( 'NONE', #13415 ) ;
#6658 = VECTOR ( 'NONE', #18814, 1000.000000000000114 ) ;
#6659 = VERTEX_POINT ( 'NONE', #14981 ) ;
#6660 = DIRECTION ( 'NONE',  ( 0.000000000000000000, -0.000000000000000000, 1.000000000000000000 ) ) ;
#6661 = ORIENTED_EDGE ( 'NONE', *, *, #12310, .T. ) ;
#6662 = DIRECTION ( 'NONE',  ( 0.000000000000000000, -0.000000000000000000, 1.000000000000000000 ) ) ;
#6663 = VECTOR ( 'NONE', #10397, 1000.000000000000000 ) ;
#6664 = VECTOR ( 'NONE', #10314, 1000.000000000000000 ) ;
#6665 = VERTEX_POINT ( 'NONE', #19606 ) ;
#6666 = CARTESIAN_POINT ( 'NONE',  ( 8.315941417683177406, -20.79840458871654363, 4.773278322869464851 ) ) ;
#6667 = CARTESIAN_POINT ( 'NONE',  ( -17.55017143803810242, 4.999999999999999112, 0.000000000000000000 ) ) ;
#6668 = EDGE_CURVE ( 'NONE', #13489, #14060, #16456, .T. ) ;
#6669 = CARTESIAN_POINT ( 'NONE',  ( -1.700193846275138032, -9.865151716929458914, 2.372704024825938340 ) ) ;
#6670 = CARTESIAN_POINT ( 'NONE',  ( 3.277163086644854229, -14.76879761173520578, 3.824673233536266537 ) ) ;
#6671 = CARTESIAN_POINT ( 'NONE',  ( -11.59030858231679417, -21.32581373872472952, 1.729004561291657138 ) ) ;
#6672 = SURFACE_STYLE_USAGE ( .BOTH. , #1958 ) ;
#6673 = EDGE_CURVE ( 'NONE', #12837, #19679, #3590, .T. ) ;
#6674 = EDGE_CURVE ( 'NONE', #4492, #2477, #19512, .T. ) ;
#6675 = CARTESIAN_POINT ( 'NONE',  ( 6.909691417683177406, -21.32581373872474373, 5.270995438708348857 ) ) ;
#6676 = DIRECTION ( 'NONE',  ( 1.000000000000000000, 0.000000000000000000, 0.000000000000000000 ) ) ;
#6677 = CARTESIAN_POINT ( 'NONE',  ( -4.659691417683178294, -22.67418626127524917, 1.729004561291651809 ) ) ;
#6678 = ORIENTED_EDGE ( 'NONE', *, *, #19139, .F. ) ;
#6679 = CARTESIAN_POINT ( 'NONE',  ( 10.55905858231679595, -20.19639159124062999, 5.231925497173373074 ) ) ;
#6680 = CARTESIAN_POINT ( 'NONE',  ( 12.62499999999998579, -20.24999999999999289, 3.146526952850934755 ) ) ;
#6681 = CARTESIAN_POINT ( 'NONE',  ( -12.62499999999998224, -20.24999999999998934, 4.291666666666698937 ) ) ;
#6682 = ORIENTED_EDGE ( 'NONE', *, *, #13605, .F. ) ;
#6683 = CARTESIAN_POINT ( 'NONE',  ( 15.06494360078803041, 10.00000000000000000, 0.000000000000000000 ) ) ;
#6684 = CARTESIAN_POINT ( 'NONE',  ( 0.000000000000000000, 9.000000000000001776, 1.000000000000000000 ) ) ;
#6685 = VECTOR ( 'NONE', #10490, 1000.000000000000000 ) ;
#6686 = VERTEX_POINT ( 'NONE', #11542 ) ;
#6687 = DIRECTION ( 'NONE',  ( 0.000000000000000000, 0.000000000000000000, 1.000000000000000000 ) ) ;
#6688 = ORIENTED_EDGE ( 'NONE', *, *, #15176, .T. ) ;
#6689 = AXIS2_PLACEMENT_3D ( 'NONE', #5220, #14533, #17783 ) ;
#6690 = CARTESIAN_POINT ( 'NONE',  ( 12.62499999999998224, -20.20698198228766529, 3.551156945995088243 ) ) ;
#6691 = ORIENTED_EDGE ( 'NONE', *, *, #15226, .T. ) ;
#6692 = CARTESIAN_POINT ( 'NONE',  ( -11.59030858231679595, -21.01515356694490322, 0.9790045612916562501 ) ) ;
#6693 = CARTESIAN_POINT ( 'NONE',  ( 13.12529397354238192, 5.014845663890295846, 4.583333333333296622 ) ) ;
#6694 = EDGE_CURVE ( 'NONE', #8351, #2802, #5474, .T. ) ;
#6695 = LINE ( 'NONE', #13065, #20178 ) ;
#6696 = CARTESIAN_POINT ( 'NONE',  ( 12.64131715375063258, -19.42598373559290792, 5.491151580003103660 ) ) ;
#6697 =( GEOMETRIC_REPRESENTATION_CONTEXT ( 3 ) GLOBAL_UNCERTAINTY_ASSIGNED_CONTEXT ( ( #16960 ) ) GLOBAL_UNIT_ASSIGNED_CONTEXT ( ( #14952, #10252, #4084 ) ) REPRESENTATION_CONTEXT ( 'NONE', 'WORKASPACE' ) );
#6698 = CYLINDRICAL_SURFACE ( 'NONE', #9682, 0.4999999999999987232 ) ;
#6699 = CARTESIAN_POINT ( 'NONE',  ( -13.84495141469777479, 4.232546442235974204, 5.040078719623224401 ) ) ;
#6700 = CARTESIAN_POINT ( 'NONE',  ( 7.371558582316795949, -19.49999999999998934, 3.449312527122348371 ) ) ;
#6701 = CARTESIAN_POINT ( 'NONE',  ( -12.62499999998404121, -20.24999999996810729, 2.793053905886972998 ) ) ;
#6702 = CARTESIAN_POINT ( 'NONE',  ( -5.309058582316795949, -23.80360840875935935, 1.768074502826626260 ) ) ;
#6703 = VECTOR ( 'NONE', #19418, 1000.000000000000000 ) ;
#6704 = PLANE ( 'NONE',  #20437 ) ;
#6705 = DIRECTION ( 'NONE',  ( 1.000000000000000000, 2.312964634635731617E-15, 0.000000000000000000 ) ) ;
#6706 = EDGE_CURVE ( 'NONE', #18372, #6318, #5163, .T. ) ;
#6707 = CARTESIAN_POINT ( 'NONE',  ( 6.902808582316795949, -22.46490103525074034, 2.520995438708341307 ) ) ;
#6708 = CARTESIAN_POINT ( 'NONE',  ( -5.878441417683177406, -23.74999999999999645, 3.449312527122335492 ) ) ;
#6709 = EDGE_LOOP ( 'NONE', ( #4232, #329, #5496, #14812 ) ) ;
#6710 = ORIENTED_EDGE ( 'NONE', *, *, #13115, .T. ) ;
#6711 = CARTESIAN_POINT ( 'NONE',  ( 13.37741471237955260, -20.12805702483293757, 4.993653275319895890 ) ) ;
#6712 = CARTESIAN_POINT ( 'NONE',  ( -23.35856191738413656, 4.999999999999999112, 1.000000000000000000 ) ) ;
#6713 = DIRECTION ( 'NONE',  ( 0.1351665943404306014, -0.9596796555888912339, 0.2464649070825229438 ) ) ;
#6714 = ORIENTED_EDGE ( 'NONE', *, *, #1172, .F. ) ;
#6715 = EDGE_LOOP ( 'NONE', ( #11744, #4665, #6742, #5589 ) ) ;
#6716 = LINE ( 'NONE', #19581, #12114 ) ;
#6717 = CARTESIAN_POINT ( 'NONE',  ( -30.00000000000000000, 10.00000000000000000, 1.000000000000000000 ) ) ;
#6718 = VECTOR ( 'NONE', #11454, 1000.000000000000000 ) ;
#6719 = CARTESIAN_POINT ( 'NONE',  ( 13.37741471237955260, -20.12805702483293757, 4.993653275319895890 ) ) ;
#6720 = EDGE_CURVE ( 'NONE', #9631, #11562, #13112, .T. ) ;
#6721 = VECTOR ( 'NONE', #5872, 1000.000000000000000 ) ;
#6722 = EDGE_CURVE ( 'NONE', #1137, #19645, #6744, .T. ) ;
#6723 = FACE_BOUND ( 'NONE', #14823, .T. ) ;
#6724 = DIRECTION ( 'NONE',  ( 0.000000000000000000, -0.000000000000000000, 1.000000000000000000 ) ) ;
#6725 = CARTESIAN_POINT ( 'NONE',  ( -13.11017182064853159, 4.251176942750957366, 5.979809059808775196 ) ) ;
#6726 = CARTESIAN_POINT ( 'NONE',  ( 9.246558582316794173, -21.94931252712234482, 5.250000000000000888 ) ) ;
#6727 = DIRECTION ( 'NONE',  ( 1.000000000000000000, 0.000000000000000000, 0.000000000000000000 ) ) ;
#6728 = CARTESIAN_POINT ( 'NONE',  ( 13.09532840572934376, 3.501584489333809724, 5.996774842915142401 ) ) ;
#6729 = CARTESIAN_POINT ( 'NONE',  ( -2.203959450683124377, -9.262433282444222371, 2.410528873095051594 ) ) ;
#6730 = ORIENTED_EDGE ( 'NONE', *, *, #13240, .T. ) ;
#6731 = AXIS2_PLACEMENT_3D ( 'NONE', #14022, #20626, #20431 ) ;
#6732 = CARTESIAN_POINT ( 'NONE',  ( -13.86106797245302147, 4.296432608878145487, 5.947261916831099171 ) ) ;
#6733 = CARTESIAN_POINT ( 'NONE',  ( 5.683390479346035029, 0.000000000000000000, 1.000000000000000000 ) ) ;
#6734 = EDGE_CURVE ( 'NONE', #607, #1583, #8611, .T. ) ;
#6735 = VECTOR ( 'NONE', #19807, 1000.000000000000000 ) ;
#6736 = CARTESIAN_POINT ( 'NONE',  ( 9.347191417683177406, -21.22443879296941915, 1.770995438708345748 ) ) ;
#6737 = CARTESIAN_POINT ( 'NONE',  ( -7.746558582316795949, -21.94931252712234127, 4.499999999999999112 ) ) ;
#6738 = ORIENTED_EDGE ( 'NONE', *, *, #17284, .F. ) ;
#6739 = CARTESIAN_POINT ( 'NONE',  ( 13.86436316834274329, 3.712840001305938831, 6.736817769197426031 ) ) ;
#6740 = CARTESIAN_POINT ( 'NONE',  ( 13.06655316810189227, 2.048434989138931961, 5.965524842914772030 ) ) ;
#6741 = CARTESIAN_POINT ( 'NONE',  ( -0.1250000000000001110, 11.64110105645932691, 10.00000000000000000 ) ) ;
#6742 = ORIENTED_EDGE ( 'NONE', *, *, #17190, .T. ) ;
#6743 = ORIENTED_EDGE ( 'NONE', *, *, #12092, .T. ) ;
#6744 = LINE ( 'NONE', #6838, #10114 ) ;
#6745 = FACE_OUTER_BOUND ( 'NONE', #20459, .T. ) ;
#6746 = EDGE_CURVE ( 'NONE', #8535, #68, #3903, .T. ) ;
#6747 = FACE_OUTER_BOUND ( 'NONE', #12821, .T. ) ;
#6748 = AXIS2_PLACEMENT_3D ( 'NONE', #18722, #3965, #2602 ) ;
#6749 = DIRECTION ( 'NONE',  ( -0.000000000000000000, 0.000000000000000000, -1.000000000000000000 ) ) ;
#6750 = CARTESIAN_POINT ( 'NONE',  ( 2.742252025265078608, -15.06657917462210605, 2.958534504914692942 ) ) ;
#6751 = DIRECTION ( 'NONE',  ( 1.000000000000000000, -0.000000000000000000, -0.000000000000000000 ) ) ;
#6752 = DIRECTION ( 'NONE',  ( 0.4999999999999948930, 0.8660254037844415942, -0.000000000000000000 ) ) ;
#6753 = DIRECTION ( 'NONE',  ( 0.000000000000000000, -1.000000000000000000, 0.000000000000000000 ) ) ;
#6754 = CARTESIAN_POINT ( 'NONE',  ( -14.49999999999999645, -21.00000000000000355, 1.000000000000000000 ) ) ;
#6755 = CARTESIAN_POINT ( 'NONE',  ( -7.371558582316794173, -20.24999999999999289, 3.449312527122348371 ) ) ;
#6756 = CARTESIAN_POINT ( 'NONE',  ( -3.549867680106858714, -10.29705900472337632, 2.118856410057032402 ) ) ;
#6757 = ORIENTED_EDGE ( 'NONE', *, *, #18090, .F. ) ;
#6758 = CARTESIAN_POINT ( 'NONE',  ( -13.06641424290328501, 2.791419266617020334, 5.231470106674447784 ) ) ;
#6759 = CARTESIAN_POINT ( 'NONE',  ( -5.215308582316795949, -23.02099543870833998, 3.136473910504556262 ) ) ;
#6760 = EDGE_CURVE ( 'NONE', #9631, #19648, #7155, .T. ) ;
#6761 = CARTESIAN_POINT ( 'NONE',  ( -9.534691417683177406, -20.22900456129164581, 2.825813738724747726 ) ) ;
#6762 = ORIENTED_EDGE ( 'NONE', *, *, #2620, .F. ) ;
#6763 = CARTESIAN_POINT ( 'NONE',  ( 13.53317008522746434, -11.51241069598931510, 4.909333296715523431 ) ) ;
#6764 = CARTESIAN_POINT ( 'NONE',  ( -2.061130159782011972, 0.000000000000000000, 1.000000000000000000 ) ) ;
#6765 = ORIENTED_EDGE ( 'NONE', *, *, #9673, .T. ) ;
#6766 = ORIENTED_EDGE ( 'NONE', *, *, #6561, .F. ) ;
#6767 = AXIS2_PLACEMENT_3D ( 'NONE', #386, #19325, #14704 ) ;
#6768 = CARTESIAN_POINT ( 'NONE',  ( -1.437849085826860884, 0.000000000000000000, 1.000000000000000000 ) ) ;
#6769 = ORIENTED_EDGE ( 'NONE', *, *, #14801, .F. ) ;
#6770 = DIRECTION ( 'NONE',  ( -1.000000000000000000, 0.000000000000000000, 0.000000000000000000 ) ) ;
#6771 = EDGE_LOOP ( 'NONE', ( #1414, #13488, #8380, #10223 ) ) ;
#6772 = CARTESIAN_POINT ( 'NONE',  ( 4.753441417683176518, -21.94931252712233061, 1.749999999999998446 ) ) ;
#6773 = CARTESIAN_POINT ( 'NONE',  ( 14.50000000000000000, -20.99999999999998934, 1.000000000000000000 ) ) ;
#6774 = CARTESIAN_POINT ( 'NONE',  ( -2.616536356806028696, -10.07836329504444706, 2.620076000170431296 ) ) ;
#6775 = CARTESIAN_POINT ( 'NONE',  ( 0.000000000000000000, 16.00000000000000000, 1.000000000000000000 ) ) ;
#6776 = CARTESIAN_POINT ( 'NONE',  ( -5.215308582316794173, -23.77099543870833998, 2.825813738724734847 ) ) ;
#6777 = VECTOR ( 'NONE', #20541, 1000.000000000000000 ) ;
#6778 = CARTESIAN_POINT ( 'NONE',  ( 9.722191417683177406, -20.27099543870833998, 4.275561207030583510 ) ) ;
#6779 = LINE ( 'NONE', #13244, #870 ) ;
#6780 = CARTESIAN_POINT ( 'NONE',  ( -10.19094141768317741, -22.74294823697955081, 4.171265325393542334 ) ) ;
#6781 = ORIENTED_EDGE ( 'NONE', *, *, #17722, .F. ) ;
#6782 = CARTESIAN_POINT ( 'NONE',  ( 8.777808582316797725, -19.52099543870833642, 2.413778621189609286 ) ) ;
#6783 = CARTESIAN_POINT ( 'NONE',  ( 12.68288333306630378, -17.32689168014509207, 5.548858176248425700 ) ) ;
#6784 = CARTESIAN_POINT ( 'NONE',  ( -13.11862022235054503, 3.927821228673052723, 6.755987001683414483 ) ) ;
#6785 = ORIENTED_EDGE ( 'NONE', *, *, #5809, .F. ) ;
#6786 = EDGE_CURVE ( 'NONE', #14414, #17290, #10081, .T. ) ;
#6787 = DIRECTION ( 'NONE',  ( 0.000000000000000000, 1.000000000000000000, 0.000000000000000000 ) ) ;
#6788 = PLANE ( 'NONE',  #5649 ) ;
#6789 = ORIENTED_EDGE ( 'NONE', *, *, #12310, .F. ) ;
#6790 = CARTESIAN_POINT ( 'NONE',  ( 0.000000000000000000, 0.000000000000000000, 0.000000000000000000 ) ) ;
#6791 = ORIENTED_EDGE ( 'NONE', *, *, #150, .F. ) ;
#6792 = CIRCLE ( 'NONE', #20161, 10.00000000000000000 ) ;
#6793 = CARTESIAN_POINT ( 'NONE',  ( 12.76142888321704305, -19.96053231526083138, 3.532471378156773589 ) ) ;
#6794 = VERTEX_POINT ( 'NONE', #16353 ) ;
#6795 = CARTESIAN_POINT ( 'NONE',  ( 23.31633994409548549, 11.64110105645932691, 10.00000000000000000 ) ) ;
#6796 = CARTESIAN_POINT ( 'NONE',  ( 13.12424783836753228, 4.962015837561366993, 5.328858059679200565 ) ) ;
#6797 = DIRECTION ( 'NONE',  ( 0.000000000000000000, -0.000000000000000000, 1.000000000000000000 ) ) ;
#6798 = CARTESIAN_POINT ( 'NONE',  ( 12.64931222250080545, -19.02223276370786209, 5.512399842915133519 ) ) ;
#6799 = DIRECTION ( 'NONE',  ( -0.000000000000000000, -0.000000000000000000, -1.000000000000000000 ) ) ;
#6800 = CARTESIAN_POINT ( 'NONE',  ( -13.37503071710846925, -20.24844878602346299, 4.564052989354591361 ) ) ;
#6801 = CARTESIAN_POINT ( 'NONE',  ( 9.246558582316795949, -21.94931252712234127, 6.000000000000001776 ) ) ;
#6802 = CARTESIAN_POINT ( 'NONE',  ( -13.15498530132288479, 5.764257716805535559, 4.333333333333380999 ) ) ;
#6803 = CARTESIAN_POINT ( 'NONE',  ( -7.184058582316795949, -20.26807450282662160, 1.696391591240633101 ) ) ;
#6804 = CARTESIAN_POINT ( 'NONE',  ( -17.05017143803810242, 0.000000000000000000, 1.000000000000000000 ) ) ;
#6805 = CARTESIAN_POINT ( 'NONE',  ( 25.54469207716615031, 4.999999999999999112, 0.000000000000000000 ) ) ;
#6806 = ADVANCED_FACE ( 'NONE', ( #8719 ), #10280, .F. ) ;
#6807 = CARTESIAN_POINT ( 'NONE',  ( 8.215308582316795949, -23.02099543870833998, 3.136473910504556262 ) ) ;
#6808 = CARTESIAN_POINT ( 'NONE',  ( -4.659691417683178294, -22.67418626127524917, 1.729004561291651587 ) ) ;
#6809 = ORIENTED_EDGE ( 'NONE', *, *, #8012, .T. ) ;
#6810 = ORIENTED_EDGE ( 'NONE', *, *, #82, .T. ) ;
#6811 = CARTESIAN_POINT ( 'NONE',  ( 13.37499999999998579, -20.24999999999999289, 3.146526952850934755 ) ) ;
#6812 = CARTESIAN_POINT ( 'NONE',  ( -7.500000000000000888, -9.999999999999992895, 2.500000000000000000 ) ) ;
#6813 = VERTEX_POINT ( 'NONE', #2129 ) ;
#6814 = LINE ( 'NONE', #14651, #17473 ) ;
#6815 = EDGE_CURVE ( 'NONE', #6038, #10907, #17791, .T. ) ;
#6816 = ADVANCED_FACE ( 'NONE', ( #11746 ), #19921, .F. ) ;
#6817 = DIRECTION ( 'NONE',  ( 0.000000000000000000, 0.000000000000000000, -1.000000000000000000 ) ) ;
#6818 = DIRECTION ( 'NONE',  ( 0.000000000000000000, 1.000000000000000000, -0.000000000000000000 ) ) ;
#6819 = CARTESIAN_POINT ( 'NONE',  ( 13.40621837757088564, -18.67347193267085714, 5.505367199623145247 ) ) ;
#6820 = LINE ( 'NONE', #3092, #18221 ) ;
#6821 = CARTESIAN_POINT ( 'NONE',  ( 3.594802210173583035, -11.77224174634763898, 3.247712807842289884 ) ) ;
#6822 = PLANE ( 'NONE',  #13719 ) ;
#6823 = CARTESIAN_POINT ( 'NONE',  ( -12.62933427970994238, -19.28111887465110996, 4.754790882998214840 ) ) ;
#6824 = CARTESIAN_POINT ( 'NONE',  ( 7.371558582316794173, -20.24999999999999289, 3.449312527122348371 ) ) ;
#6825 = FACE_OUTER_BOUND ( 'NONE', #18265, .T. ) ;
#6826 = CARTESIAN_POINT ( 'NONE',  ( 13.12424783836753228, 4.962015837561366993, 5.328858059679200565 ) ) ;
#6827 = CARTESIAN_POINT ( 'NONE',  ( -2.579281110863027582, -9.822567596814183233, 2.554382554832406615 ) ) ;
#6828 = CARTESIAN_POINT ( 'NONE',  ( 7.652808582316796837, -21.53509896474924901, 4.479004561291659137 ) ) ;
#6829 = EDGE_CURVE ( 'NONE', #3840, #11512, #5574, .T. ) ;
#6830 = CARTESIAN_POINT ( 'NONE',  ( 8.690941417683177406, -23.27327832286946219, 4.701595411283453707 ) ) ;
#6831 = CARTESIAN_POINT ( 'NONE',  ( -7.559058582316795949, -21.25705176302045274, 4.171265325393551215 ) ) ;
#6832 = ORIENTED_EDGE ( 'NONE', *, *, #1609, .T. ) ;
#6833 = CARTESIAN_POINT ( 'NONE',  ( 13.89730118381875279, 5.376209782841177898, 6.083536567043803522 ) ) ;
#6834 = CARTESIAN_POINT ( 'NONE',  ( 12.64691428603184242, -19.14332855539073464, 5.509795676248469221 ) ) ;
#6835 = CARTESIAN_POINT ( 'NONE',  ( -13.12499999999999467, 5.000000000000047073, 3.999999999999996447 ) ) ;
#6836 = ORIENTED_EDGE ( 'NONE', *, *, #8253, .T. ) ;
#6837 = VERTEX_POINT ( 'NONE', #13207 ) ;
#6838 = CARTESIAN_POINT ( 'NONE',  ( 0.000000000000000000, 9.000000000000001776, 1.000000000000000000 ) ) ;
#6839 = CARTESIAN_POINT ( 'NONE',  ( -17.55017143803810242, 9.000000000000001776, 1.000000000000000000 ) ) ;
#6840 = DIRECTION ( 'NONE',  ( 8.673617379884033500E-16, -1.000000000000000000, 0.000000000000000000 ) ) ;
#6841 = EDGE_CURVE ( 'NONE', #20320, #16909, #11637, .T. ) ;
#6842 = DIRECTION ( 'NONE',  ( 0.000000000000000000, -0.000000000000000000, 1.000000000000000000 ) ) ;
#6843 = CARTESIAN_POINT ( 'NONE',  ( 1.991511895312070957, -10.01421418592441448, 1.660986244685804136 ) ) ;
#6844 = DIRECTION ( 'NONE',  ( 1.000000000000000000, 0.000000000000000000, 0.000000000000000000 ) ) ;
#6845 = DIRECTION ( 'NONE',  ( 1.000000000000000000, 0.000000000000000000, 0.000000000000000000 ) ) ;
#6846 = CARTESIAN_POINT ( 'NONE',  ( 13.26156167763900307, -20.51872823783367750, 3.464319252107387115 ) ) ;
#6847 = DIRECTION ( 'NONE',  ( -1.000000000000000000, 6.938893903907222067E-15, 0.000000000000000000 ) ) ;
#6848 = CARTESIAN_POINT ( 'NONE',  ( -6.715308582316794173, -23.77099543870833998, 2.825813738724734847 ) ) ;
#6849 = CARTESIAN_POINT ( 'NONE',  ( -1.932703420524435112, -8.381852853175612239, 2.376993210252662969 ) ) ;
#6850 = EDGE_LOOP ( 'NONE', ( #526, #8361, #3185, #13108 ) ) ;
#6851 = CARTESIAN_POINT ( 'NONE',  ( -12.64197948789552051, -18.64253586127677309, 4.770532606674187548 ) ) ;
#6852 = CARTESIAN_POINT ( 'NONE',  ( -5.777808582316794173, -20.27099543870833642, 2.724438792969431589 ) ) ;
#6853 = ADVANCED_FACE ( 'NONE', ( #8512 ), #14881, .T. ) ;
#6854 = CARTESIAN_POINT ( 'NONE',  ( -7.847191417683176518, -21.22443879296941915, 1.770995438708345748 ) ) ;
#6855 = ORIENTED_EDGE ( 'NONE', *, *, #6841, .T. ) ;
#6856 = EDGE_CURVE ( 'NONE', #8532, #14522, #9027, .T. ) ;
#6857 = CARTESIAN_POINT ( 'NONE',  ( 13.38210008768272630, -19.14144557202113006, 4.745270796715706396 ) ) ;
#6859 = DIRECTION ( 'NONE',  ( 0.000000000000000000, 0.000000000000000000, 1.000000000000000000 ) ) ;
#6858 = VECTOR ( 'NONE', #20666, 1000.000000000000000 ) ;
#6860 = ORIENTED_EDGE ( 'NONE', *, *, #9410, .T. ) ;
#6861 = VERTEX_POINT ( 'NONE', #15192 ) ;
#6862 = LINE ( 'NONE', #19843, #9420 ) ;
#6863 = VERTEX_POINT ( 'NONE', #6099 ) ;
#6864 = DIRECTION ( 'NONE',  ( 0.000000000000000000, -1.000000000000000000, 0.000000000000000000 ) ) ;
#6865 = VECTOR ( 'NONE', #13859, 1000.000000000000114 ) ;
#6866 = ORIENTED_EDGE ( 'NONE', *, *, #18654, .T. ) ;
#6867 = CARTESIAN_POINT ( 'NONE',  ( 5.597191417683177406, -22.77556120703057729, 5.229004561291656472 ) ) ;
#6868 = EDGE_CURVE ( 'NONE', #20635, #9650, #10701, .T. ) ;
#6869 = FACE_OUTER_BOUND ( 'NONE', #7693, .T. ) ;
#6870 = FACE_OUTER_BOUND ( 'NONE', #1511, .T. ) ;
#6871 = FACE_OUTER_BOUND ( 'NONE', #14204, .T. ) ;
#6872 = CARTESIAN_POINT ( 'NONE',  ( -6.059058582316793284, -20.72672167713054137, 4.701595411283463477 ) ) ;
#6873 = CARTESIAN_POINT ( 'NONE',  ( -15.49999999999999822, -22.99999999999999289, 4.000000000000000000 ) ) ;
#6874 = CARTESIAN_POINT ( 'NONE',  ( 8.597191417683177406, -22.77556120703057729, 5.229004561291655584 ) ) ;
#6875 = DIRECTION ( 'NONE',  ( 0.000000000000000000, 0.000000000000000000, -1.000000000000000000 ) ) ;
#6876 = CARTESIAN_POINT ( 'NONE',  ( -5.972191417683178294, -22.97900456129165292, 3.035098964749240125 ) ) ;
#6877 = CARTESIAN_POINT ( 'NONE',  ( -7.184058582316795949, -20.26807450282662160, 1.696391591240633101 ) ) ;
#6878 = ORIENTED_EDGE ( 'NONE', *, *, #9108, .F. ) ;
#6879 = CARTESIAN_POINT ( 'NONE',  ( 12.62745083560477966, -20.12623280195927933, 5.001038150054709419 ) ) ;
#6880 = CARTESIAN_POINT ( 'NONE',  ( -13.08107971211413378, 2.032025461757085427, 6.715204579155630960 ) ) ;
#6881 = ORIENTED_EDGE ( 'NONE', *, *, #20226, .T. ) ;
#6882 = LINE ( 'NONE', #11792, #1280 ) ;
#6883 = FACE_OUTER_BOUND ( 'NONE', #12490, .T. ) ;
#6884 = ORIENTED_EDGE ( 'NONE', *, *, #20030, .F. ) ;
#6885 = VECTOR ( 'NONE', #11482, 1000.000000000000000 ) ;
#6886 = PRODUCT_CONTEXT ( 'NONE', #7340, 'mechanical' ) ;
#6887 = ORIENTED_EDGE ( 'NONE', *, *, #5137, .T. ) ;
#6888 = CARTESIAN_POINT ( 'NONE',  ( 2.583953725994688533, -9.847075946378776479, 2.560676788604062004 ) ) ;
#6889 = EDGE_LOOP ( 'NONE', ( #10906, #5114, #6789, #8847, #5812, #2727 ) ) ;
#6890 = DIRECTION ( 'NONE',  ( -1.000000000000000000, 0.000000000000000000, 0.000000000000000000 ) ) ;
#6891 = EDGE_CURVE ( 'NONE', #4104, #12575, #13614, .T. ) ;
#6892 = CARTESIAN_POINT ( 'NONE',  ( 13.10252221513633941, 3.864871864382954048, 6.004587342915129966 ) ) ;
#6893 = LINE ( 'NONE', #513, #11142 ) ;
#6894 = AXIS2_PLACEMENT_3D ( 'NONE', #13588, #9202, #20411 ) ;
#6895 = CARTESIAN_POINT ( 'NONE',  ( 13.15498530132288479, 5.764257716805535559, 2.999999999999999556 ) ) ;
#6896 = CARTESIAN_POINT ( 'NONE',  ( -2.693754455098655409, -9.955255285363838524, 2.600628789231445470 ) ) ;
#6897 = AXIS2_PLACEMENT_3D ( 'NONE', #14475, #17828, #7995 ) ;
#6898 = CARTESIAN_POINT ( 'NONE',  ( 10.55905858231679595, -20.19639159124062999, 5.231925497173373074 ) ) ;
#6899 = CARTESIAN_POINT ( 'NONE',  ( -12.62503117662529739, -20.24842558042254836, 4.565011198945062354 ) ) ;
#6900 = CARTESIAN_POINT ( 'NONE',  ( -5.027808582316795949, -24.47900456129166358, 4.586221378810390270 ) ) ;
#6901 = DIRECTION ( 'NONE',  ( 1.000000000000000000, 0.000000000000000000, -0.000000000000000000 ) ) ;
#6902 = FACE_OUTER_BOUND ( 'NONE', #13845, .T. ) ;
#6903 = CARTESIAN_POINT ( 'NONE',  ( 8.965308582316795949, -20.97900456129165647, 3.863526089495444626 ) ) ;
#6904 = LINE ( 'NONE', #16521, #6319 ) ;
#6905 = EDGE_LOOP ( 'NONE', ( #17854, #1967, #2880, #17072 ) ) ;
#6906 = ORIENTED_EDGE ( 'NONE', *, *, #184, .F. ) ;
#6907 = CARTESIAN_POINT ( 'NONE',  ( 13.87470602645761986, 4.985154336109792972, 4.791666666666685614 ) ) ;
#6908 = EDGE_CURVE ( 'NONE', #19548, #16322, #18862, .T. ) ;
#6909 = CARTESIAN_POINT ( 'NONE',  ( 0.000000000000000000, 10.00000000000000000, 1.000000000000000000 ) ) ;
#6910 = ORIENTED_EDGE ( 'NONE', *, *, #20652, .F. ) ;
#6911 = CARTESIAN_POINT ( 'NONE',  ( -13.49999999999998401, -25.49999999999999645, 4.000000000000000000 ) ) ;
#6912 = CARTESIAN_POINT ( 'NONE',  ( -4.250698171653726654, 10.00000000000000000, 1.000000000000000000 ) ) ;
#6913 = CARTESIAN_POINT ( 'NONE',  ( -0.000000000000000000, 10.00000000000000000, 0.000000000000000000 ) ) ;
#6914 = CARTESIAN_POINT ( 'NONE',  ( 13.37503071710846925, -20.24844878602346299, 4.564052989354591361 ) ) ;
#6915 = CARTESIAN_POINT ( 'NONE',  ( 0.000000000000000000, 10.00000000000000000, 1.000000000000000000 ) ) ;
#6916 = CARTESIAN_POINT ( 'NONE',  ( 1.717920576997000737, -9.114924032904250240, 2.372645551019823884 ) ) ;
#6917 =( GEOMETRIC_REPRESENTATION_CONTEXT ( 3 ) GLOBAL_UNCERTAINTY_ASSIGNED_CONTEXT ( ( #1282 ) ) GLOBAL_UNIT_ASSIGNED_CONTEXT ( ( #8702, #16748, #7238 ) ) REPRESENTATION_CONTEXT ( 'NONE', 'WORKASPACE' ) );
#6918 = EDGE_CURVE ( 'NONE', #19819, #10249, #10809, .T. ) ;
#6919 = CARTESIAN_POINT ( 'NONE',  ( 1.852280067228949445, -9.126254559850970338, 1.625555456689752321 ) ) ;
#6920 = CARTESIAN_POINT ( 'NONE',  ( -12.62500797102436678, -19.49959746326937093, 4.516621614626514791 ) ) ;
#6921 = CARTESIAN_POINT ( 'NONE',  ( 5.684058582316794173, -20.79840458871652942, 2.226721677130544030 ) ) ;
#6922 = CARTESIAN_POINT ( 'NONE',  ( -5.999999999999999112, -7.500000000000047073, 8.999999999999998224 ) ) ;
#6923 = CARTESIAN_POINT ( 'NONE',  ( 12.64691428603184242, -19.14332855539073464, 5.509795676248469221 ) ) ;
#6924 = CARTESIAN_POINT ( 'NONE',  ( -3.277163086644854229, -14.76879761173520578, 3.824673233536266537 ) ) ;
#6925 = EDGE_CURVE ( 'NONE', #431, #1458, #13925, .T. ) ;
#6926 = CARTESIAN_POINT ( 'NONE',  ( 6.809058582316796837, -22.74294823697954016, 2.828734674606448785 ) ) ;
#6928 = ADVANCED_FACE ( 'NONE', ( #8921 ), #17073, .T. ) ;
#6927 = AXIS2_PLACEMENT_3D ( 'NONE', #9749, #6612, #19071 ) ;
#6929 = CARTESIAN_POINT ( 'NONE',  ( 9.815941417683177406, -20.79840458871654363, 4.773278322869464851 ) ) ;
#6930 = CARTESIAN_POINT ( 'NONE',  ( -7.840308582316795949, -22.36352608949544418, 4.520995438708343528 ) ) ;
#6931 = ORIENTED_EDGE ( 'NONE', *, *, #5565, .T. ) ;
#6932 = CARTESIAN_POINT ( 'NONE',  ( 13.11862022235054503, 3.927821228673052723, 6.755987001683414483 ) ) ;
#6933 = CARTESIAN_POINT ( 'NONE',  ( 12.63036675113625407, -19.22897906761645004, 4.757923088130392664 ) ) ;
#6934 = CARTESIAN_POINT ( 'NONE',  ( -5.999999999999999112, -7.500000000000047073, 2.000000000000000000 ) ) ;
#6935 = EDGE_LOOP ( 'NONE', ( #13465, #13971, #19757, #1107 ) ) ;
#6936 = VERTEX_POINT ( 'NONE', #5988 ) ;
#6937 = DIRECTION ( 'NONE',  ( -0.000000000000000000, -0.000000000000000000, -1.000000000000000000 ) ) ;
#6938 = DIRECTION ( 'NONE',  ( 0.000000000000000000, 1.000000000000000000, -0.000000000000000000 ) ) ;
#6939 = CARTESIAN_POINT ( 'NONE',  ( 6.063547257480584207, 0.000000000000000000, 1.000000000000000000 ) ) ;
#6940 = EDGE_CURVE ( 'NONE', #3190, #1434, #8826, .T. ) ;
#6941 = DIRECTION ( 'NONE',  ( 0.000000000000000000, 0.000000000000000000, -1.000000000000000000 ) ) ;
#6942 = CARTESIAN_POINT ( 'NONE',  ( 2.817596665886821672, -11.50588678273290988, 2.986692549455723267 ) ) ;
#6943 = LINE ( 'NONE', #7056, #19456 ) ;
#6944 = AXIS2_PLACEMENT_3D ( 'NONE', #5215, #15147, #6890 ) ;
#6945 = DIRECTION ( 'NONE',  ( 0.000000000000000000, 1.000000000000000000, -0.000000000000000000 ) ) ;
#6946 = VECTOR ( 'NONE', #603, 1000.000000000000000 ) ;
#6947 =( BOUNDED_CURVE ( )  B_SPLINE_CURVE ( 3, ( #5071, #18995, #4651, #11448 ),
 .UNSPECIFIED., .F., .T. ) 
 B_SPLINE_CURVE_WITH_KNOTS ( ( 4, 4 ),
 ( 0.001172421487176120289, 0.001187255941418635012 ),
 .UNSPECIFIED. ) 
 CURVE ( )  GEOMETRIC_REPRESENTATION_ITEM ( )  RATIONAL_B_SPLINE_CURVE ( ( 0.9999999999999996669, 0.9870550161812248202, 0.9743613912715525238, 0.9619191252709827777 ) ) 
 REPRESENTATION_ITEM ( '' )  );
#6948 = CARTESIAN_POINT ( 'NONE',  ( 12.69334382635811487, -20.46623033821147786, 3.541734007794558270 ) ) ;
#6949 = PLANE ( 'NONE',  #20682 ) ;
#6950 = CARTESIAN_POINT ( 'NONE',  ( -10.37155858231679417, -20.24999999999999289, 3.449312527122348371 ) ) ;
#6951 = CARTESIAN_POINT ( 'NONE',  ( -1.884282074604925583, -8.375506800461993251, 2.375363417140690547 ) ) ;
#6952 = ORIENTED_EDGE ( 'NONE', *, *, #3802, .F. ) ;
#6953 = CARTESIAN_POINT ( 'NONE',  ( -13.40368151590352497, -18.05158344687463412, 4.768708296715732153 ) ) ;
#6954 = CARTESIAN_POINT ( 'NONE',  ( -8.027808582316792396, -23.72900456129165647, 4.275561207030568411 ) ) ;
#6955 = CARTESIAN_POINT ( 'NONE',  ( -5.128441417683177406, -20.24999999999999289, 3.550687472877664952 ) ) ;
#6956 = EDGE_LOOP ( 'NONE', ( #3180, #10242, #1836, #4282, #9720, #7102 ) ) ;
#6957 = CARTESIAN_POINT ( 'NONE',  ( 13.42766088059286922, -16.84062553004338625, 4.794749963382423985 ) ) ;
#6958 = CARTESIAN_POINT ( 'NONE',  ( -22.06633994409548194, 10.00000000000000000, 0.000000000000000000 ) ) ;
#6959 = VERTEX_POINT ( 'NONE', #10592 ) ;
#6960 = EDGE_CURVE ( 'NONE', #15703, #5289, #14032, .T. ) ;
#6961 = VERTEX_POINT ( 'NONE', #7358 ) ;
#6962 = FACE_OUTER_BOUND ( 'NONE', #18728, .T. ) ;
#6963 = VECTOR ( 'NONE', #19028, 1000.000000000000000 ) ;
#6964 = VERTEX_POINT ( 'NONE', #20225 ) ;
#6965 = LINE ( 'NONE', #10105, #10102 ) ;
#6966 = AXIS2_PLACEMENT_3D ( 'NONE', #19561, #5526, #16408 ) ;
#6967 = VECTOR ( 'NONE', #9287, 1000.000000000000000 ) ;
#6968 = ORIENTED_EDGE ( 'NONE', *, *, #11128, .F. ) ;
#6969 = CARTESIAN_POINT ( 'NONE',  ( 7.190941417683176518, -23.27327832286946219, 4.701595411283453707 ) ) ;
#6970 = LINE ( 'NONE', #6773, #7663 ) ;
#6971 = EDGE_CURVE ( 'NONE', #11489, #5953, #20020, .T. ) ;
#6972 = EDGE_CURVE ( 'NONE', #5711, #7723, #10494, .T. ) ;
#6973 = PLANE ( 'NONE',  #15324 ) ;
#6974 = VECTOR ( 'NONE', #16486, 1000.000000000000000 ) ;
#6975 = CARTESIAN_POINT ( 'NONE',  ( 1.126276606324276619, -8.364917468222230923, 2.372643865078341019 ) ) ;
#6976 = DIRECTION ( 'NONE',  ( 0.000000000000000000, 1.000000000000000000, 0.000000000000000000 ) ) ;
#6977 = CARTESIAN_POINT ( 'NONE',  ( 13.90439735423812273, 5.734566389025032684, 4.166666666666765551 ) ) ;
#6978 = VECTOR ( 'NONE', #1624, 1000.000000000000000 ) ;
#6979 = CARTESIAN_POINT ( 'NONE',  ( 13.50000000000000178, 5.000000000000047962, 2.000000000000000000 ) ) ;
#6980 = CIRCLE ( 'NONE', #19353, 10.00000000000000000 ) ;
#6981 = CARTESIAN_POINT ( 'NONE',  ( 10.56594141768317741, -22.67126532539353789, 2.757051763020445634 ) ) ;
#6982 = DIRECTION ( 'NONE',  ( 1.000000000000000000, -1.734723475976807094E-15, 0.000000000000000000 ) ) ;
#6983 = CARTESIAN_POINT ( 'NONE',  ( -9.065941417683177406, -22.67126532539353789, 2.757051763020445634 ) ) ;
#6984 = CARTESIAN_POINT ( 'NONE',  ( -8.215308582316795949, -24.52099543870834708, 2.515153566944913432 ) ) ;
#6985 = ORIENTED_EDGE ( 'NONE', *, *, #12299, .F. ) ;
#6986 = CARTESIAN_POINT ( 'NONE',  ( 13.09293046926041626, 3.380488697651010011, 5.994170676248444352 ) ) ;
#6987 = CARTESIAN_POINT ( 'NONE',  ( -13.15498530132288479, 5.764257716805535559, 3.666666666666500873 ) ) ;
#6988 = ORIENTED_EDGE ( 'NONE', *, *, #15695, .F. ) ;
#6989 = DIRECTION ( 'NONE',  ( 1.000000000000000000, 0.000000000000000000, -0.000000000000000000 ) ) ;
#6990 = LINE ( 'NONE', #19651, #16671 ) ;
#6991 = EDGE_LOOP ( 'NONE', ( #3379, #5389, #2714, #3963 ) ) ;
#6992 = VECTOR ( 'NONE', #15533, 1000.000000000000000 ) ;
#6993 = AXIS2_PLACEMENT_3D ( 'NONE', #8446, #17952, #10004 ) ;
#6994 = VERTEX_POINT ( 'NONE', #1182 ) ;
#6995 = VECTOR ( 'NONE', #9817, 1000.000000000000000 ) ;
#6996 = CARTESIAN_POINT ( 'NONE',  ( 13.12229871761221744, -19.89213912024655784, 3.483647646711293788 ) ) ;
#6997 = VECTOR ( 'NONE', #19538, 1000.000000000000000 ) ;
#6998 = ORIENTED_EDGE ( 'NONE', *, *, #19303, .F. ) ;
#6999 = CARTESIAN_POINT ( 'NONE',  ( 26.04469207716615031, 4.999999999999999112, 1.000000000000000000 ) ) ;
#7000 = CARTESIAN_POINT ( 'NONE',  ( 12.66369984131459070, -18.29565801360988075, 5.528024842915327142 ) ) ;
#7001 = CARTESIAN_POINT ( 'NONE',  ( -1.731569788986178304, -8.364930642962441709, 1.622647248614820015 ) ) ;
#7002 = CARTESIAN_POINT ( 'NONE',  ( 1.126276606324276619, -9.114917468222230923, 2.372643865078341019 ) ) ;
#7003 = DIRECTION ( 'NONE',  ( -0.000000000000000000, -0.000000000000000000, -1.000000000000000000 ) ) ;
#7004 = CARTESIAN_POINT ( 'NONE',  ( 13.10192273101908000, 3.834597916462216816, 6.003936301248457674 ) ) ;
#7005 = FACE_OUTER_BOUND ( 'NONE', #6889, .T. ) ;
#7006 = CARTESIAN_POINT ( 'NONE',  ( 12.52780858231679773, -24.47900456129166358, 4.586221378810390270 ) ) ;
#7007 = CARTESIAN_POINT ( 'NONE',  ( -13.15498530132288479, 5.764257716805535559, 4.916666666666649199 ) ) ;
#7008 = CARTESIAN_POINT ( 'NONE',  ( -9.722191417683177406, -19.52099543870834353, 4.586221378810406257 ) ) ;
#7009 = AXIS2_PLACEMENT_3D ( 'NONE', #17405, #5838, #7793 ) ;
#7010 = FACE_OUTER_BOUND ( 'NONE', #6771, .T. ) ;
#7011 = DIRECTION ( 'NONE',  ( -1.000000000000000000, 0.000000000000000000, 0.000000000000000000 ) ) ;
#7012 = CIRCLE ( 'NONE', #13667, 10.00000000000000000 ) ;
#7013 = EDGE_CURVE ( 'NONE', #15113, #17093, #2640, .T. ) ;
#7014 = VECTOR ( 'NONE', #8674, 1000.000000000000000 ) ;
#7015 = CARTESIAN_POINT ( 'NONE',  ( 10.37155858231679595, -20.99999999999999645, 3.449312527122348371 ) ) ;
#7016 = LINE ( 'NONE', #18305, #8996 ) ;
#7017 = EDGE_LOOP ( 'NONE', ( #11175, #9343, #2055, #3543 ) ) ;
#7018 = ORIENTED_EDGE ( 'NONE', *, *, #6288, .T. ) ;
#7019 = CARTESIAN_POINT ( 'NONE',  ( 13.85788212999909419, 4.135547564954428879, 5.982801014393342776 ) ) ;
#7020 = LINE ( 'NONE', #13387, #4440 ) ;
#7021 =( NAMED_UNIT ( * ) PLANE_ANGLE_UNIT ( ) SI_UNIT ( $, .RADIAN. ) );
#7022 = ORIENTED_EDGE ( 'NONE', *, *, #4835, .T. ) ;
#7023 = CARTESIAN_POINT ( 'NONE',  ( 7.500000000000002665, -9.999999999999991118, 1.000000000000000000 ) ) ;
#7024 = VECTOR ( 'NONE', #18509, 1000.000000000000000 ) ;
#7025 = LINE ( 'NONE', #19796, #7701 ) ;
#7026 = CARTESIAN_POINT ( 'NONE',  ( 16.37779268661489596, 0.000000000000000000, 0.000000000000000000 ) ) ;
#7027 = CARTESIAN_POINT ( 'NONE',  ( 13.85403523778986390, 3.941279508358651817, 5.991705257707216958 ) ) ;
#7028 = DIRECTION ( 'NONE',  ( -1.000000000000000000, 0.000000000000000000, 0.000000000000000000 ) ) ;
#7029 = CARTESIAN_POINT ( 'NONE',  ( 4.181771508648414404, -14.78356139460145968, 3.271079850667843125 ) ) ;
#7030 = VECTOR ( 'NONE', #7501, 1000.000000000000000 ) ;
#7031 = DIRECTION ( 'NONE',  ( -0.000000000000000000, -0.000000000000000000, -1.000000000000000000 ) ) ;
#7032 = CARTESIAN_POINT ( 'NONE',  ( -12.62917185724685254, -19.28932120903463598, 4.753410794856941735 ) ) ;
#7033 = CARTESIAN_POINT ( 'NONE',  ( 8.402808582316792396, -22.77556120703056308, 1.770995438708340197 ) ) ;
#7034 = DIRECTION ( 'NONE',  ( -0.000000000000000000, -0.000000000000000000, -1.000000000000000000 ) ) ;
#7035 = CARTESIAN_POINT ( 'NONE',  ( 13.09892531043291086, 3.683228176858501790, 6.000681092915118420 ) ) ;
#7036 = CARTESIAN_POINT ( 'NONE',  ( -2.616536356806028696, -10.07836329504444706, 2.620076000170431296 ) ) ;
#7037 = CARTESIAN_POINT ( 'NONE',  ( 9.246558582316795949, -21.94931252712234127, 4.499999999999999112 ) ) ;
#7038 = CARTESIAN_POINT ( 'NONE',  ( 7.097191417683177406, -22.77556120703057729, 5.229004561291655584 ) ) ;
#7039 = CARTESIAN_POINT ( 'NONE',  ( -13.27780858231679595, -20.27099543870833642, 2.724438792969431589 ) ) ;
#7040 = PRODUCT_DEFINITION_FORMATION_WITH_SPECIFIED_SOURCE ( 'ANY', '', #18864, .NOT_KNOWN. ) ;
#7041 = EDGE_LOOP ( 'NONE', ( #13329, #6481, #16595, #14055 ) ) ;
#7042 = CARTESIAN_POINT ( 'NONE',  ( 12.66144083004408571, -19.15973808277258073, 6.259475412489329038 ) ) ;
#7043 = CARTESIAN_POINT ( 'NONE',  ( 12.62933427970994238, -19.28111887465110996, 4.754790882998214840 ) ) ;
#7044 = CARTESIAN_POINT ( 'NONE',  ( -1.437849085826860884, 10.00000000000000000, 0.000000000000000000 ) ) ;
#7045 = EDGE_LOOP ( 'NONE', ( #1762, #7354, #1236, #11939 ) ) ;
#7046 = AXIS2_PLACEMENT_3D ( 'NONE', #20557, #1405, #4537 ) ;
#7047 = ADVANCED_FACE ( 'NONE', ( #18760 ), #12157, .T. ) ;
#7048 = VERTEX_POINT ( 'NONE', #2853 ) ;
#7049 = CARTESIAN_POINT ( 'NONE',  ( 26.69203811574920948, 1.543443504701929706E-14, 0.000000000000000000 ) ) ;
#7050 = PLANE ( 'NONE',  #18609 ) ;
#7051 = ADVANCED_FACE ( 'NONE', ( #967 ), #9227, .T. ) ;
#7052 = EDGE_CURVE ( 'NONE', #3720, #14893, #4210, .T. ) ;
#7053 = CARTESIAN_POINT ( 'NONE',  ( -12.50209451496117197, 0.000000000000000000, 0.000000000000000000 ) ) ;
#7054 = DIRECTION ( 'NONE',  ( 0.000000000000000000, 0.000000000000000000, -1.000000000000000000 ) ) ;
#7055 = CARTESIAN_POINT ( 'NONE',  ( 0.000000000000000000, -9.864917468222230923, 2.372643865078341019 ) ) ;
#7056 = CARTESIAN_POINT ( 'NONE',  ( 23.60856191738414012, 0.000000000000000000, 0.000000000000000000 ) ) ;
#7057 = LINE ( 'NONE', #17833, #10390 ) ;
#7058 = CIRCLE ( 'NONE', #1388, 0.4999999999999987232 ) ;
#7059 = CARTESIAN_POINT ( 'NONE',  ( 12.79015364697802504, -20.56461506584171062, 3.528352462579536386 ) ) ;
#7060 = DIRECTION ( 'NONE',  ( 0.000000000000000000, -1.000000000000000000, 0.000000000000000000 ) ) ;
#7061 = CARTESIAN_POINT ( 'NONE',  ( -10.27780858231679417, -20.27099543870833642, 2.724438792969431589 ) ) ;
#7062 = VECTOR ( 'NONE', #18009, 1000.000000000000000 ) ;
#7063 = CARTESIAN_POINT ( 'NONE',  ( -3.996922828336520794, -14.62728872172488437, 3.980945906412841850 ) ) ;
#7064 = ORIENTED_EDGE ( 'NONE', *, *, #19019, .F. ) ;
#7065 = CARTESIAN_POINT ( 'NONE',  ( -13.38569699238614952, -18.95980188449660986, 4.749177046715717054 ) ) ;
#7066 = CARTESIAN_POINT ( 'NONE',  ( -5.496558582316794173, -22.05068747287764452, 1.749999999999998446 ) ) ;
#7067 = CARTESIAN_POINT ( 'NONE',  ( -7.284691417683176518, -23.02099543870834353, 3.863526089495429972 ) ) ;
#7068 = VERTEX_POINT ( 'NONE', #7463 ) ;
#7069 = CARTESIAN_POINT ( 'NONE',  ( 13.85163507668220539, 3.820071372449974412, 5.989091157956555556 ) ) ;
#7070 = DIRECTION ( 'NONE',  ( 1.000000000000000000, 2.312964634635730039E-15, 0.000000000000000000 ) ) ;
#7071 = ORIENTED_EDGE ( 'NONE', *, *, #12449, .F. ) ;
#7072 = ORIENTED_EDGE ( 'NONE', *, *, #7873, .F. ) ;
#7073 = CARTESIAN_POINT ( 'NONE',  ( 0.000000000000000000, 4.999999999999999112, 1.000000000000000000 ) ) ;
#7074 = EDGE_CURVE ( 'NONE', #19964, #20408, #13823, .T. ) ;
#7075 = VERTEX_POINT ( 'NONE', #3259 ) ;
#7076 = DIRECTION ( 'NONE',  ( 0.000000000000000000, 0.000000000000000000, 1.000000000000000000 ) ) ;
#7077 = VECTOR ( 'NONE', #20092, 1000.000000000000000 ) ;
#7078 = EDGE_CURVE ( 'NONE', #19625, #20251, #12875, .T. ) ;
#7079 = EDGE_CURVE ( 'NONE', #13354, #19089, #6293, .T. ) ;
#7080 = ORIENTED_EDGE ( 'NONE', *, *, #11417, .T. ) ;
#7081 = CARTESIAN_POINT ( 'NONE',  ( 5.409691417683177406, -21.32581373872474373, 5.270995438708348857 ) ) ;
#7082 = CARTESIAN_POINT ( 'NONE',  ( -6.313547257480587760, 0.000000000000000000, 0.000000000000000000 ) ) ;
#7083 = DIRECTION ( 'NONE',  ( 0.000000000000000000, 0.000000000000000000, 1.000000000000000000 ) ) ;
#7084 = CARTESIAN_POINT ( 'NONE',  ( 2.616191246582922680, -8.630616848980537270, 2.440880773935528048 ) ) ;
#7085 = CARTESIAN_POINT ( 'NONE',  ( -4.717959273841178636, -21.72818306014730183, 5.243595146365860771 ) ) ;
#7086 = CARTESIAN_POINT ( 'NONE',  ( 12.65457057572495181, -19.50668592589112293, 6.238308001337955488 ) ) ;
#7087 = LINE ( 'NONE', #19856, #19658 ) ;
#7088 = CARTESIAN_POINT ( 'NONE',  ( 6.159691417683176518, -22.67418626127524917, 1.729004561291651809 ) ) ;
#7089 = LINE ( 'NONE', #16802, #12212 ) ;
#7090 = CARTESIAN_POINT ( 'NONE',  ( -8.597191417683177406, -22.46490103525075810, 4.479004561291653808 ) ) ;
#7091 = AXIS2_PLACEMENT_3D ( 'NONE', #8330, #1947, #3311 ) ;
#7092 = CARTESIAN_POINT ( 'NONE',  ( -5.496558582316795949, -22.05068747287764452, 0.9999999999999978906 ) ) ;
#7093 = VERTEX_POINT ( 'NONE', #16129 ) ;
#7094 = CARTESIAN_POINT ( 'NONE',  ( 12.62515856830665584, -19.49199230051052822, 4.565864671500353467 ) ) ;
#7095 = CARTESIAN_POINT ( 'NONE',  ( -13.09892531043291086, 3.683228176858501790, 6.000681092915118420 ) ) ;
#7096 = VERTEX_POINT ( 'NONE', #4930 ) ;
#7097 = DIRECTION ( 'NONE',  ( 0.000000000000000000, 0.000000000000000000, 1.000000000000000000 ) ) ;
#7098 = EDGE_CURVE ( 'NONE', #12230, #12873, #19277, .T. ) ;
#7099 = DIRECTION ( 'NONE',  ( 0.000000000000000000, 1.000000000000000000, -0.000000000000000000 ) ) ;
#7100 = ORIENTED_EDGE ( 'NONE', *, *, #594, .F. ) ;
#7101 = VECTOR ( 'NONE', #4547, 1000.000000000000000 ) ;
#7102 = ORIENTED_EDGE ( 'NONE', *, *, #8015, .F. ) ;
#7103 = LINE ( 'NONE', #1312, #14125 ) ;
#7104 = ORIENTED_EDGE ( 'NONE', *, *, #5034, .T. ) ;
#7105 = DIRECTION ( 'NONE',  ( 1.000000000000000000, 0.000000000000000000, -0.000000000000000000 ) ) ;
#7106 = VECTOR ( 'NONE', #4007, 1000.000000000000000 ) ;
#7107 = CARTESIAN_POINT ( 'NONE',  ( 13.12529397354238192, 5.014845663890295846, 4.833333333333344584 ) ) ;
#7108 = CARTESIAN_POINT ( 'NONE',  ( -3.385922596301560894, -9.481287983549590237, 1.909350115156127403 ) ) ;
#7109 = PLANE ( 'NONE',  #13321 ) ;
#7110 = CARTESIAN_POINT ( 'NONE',  ( 2.499999999999998668, -19.50000000000000000, 1.000000000000000000 ) ) ;
#7111 = EDGE_CURVE ( 'NONE', #18396, #814, #1771, .T. ) ;
#7112 = CARTESIAN_POINT ( 'NONE',  ( 13.11017182064853159, 4.251176942750957366, 5.979809059808775196 ) ) ;
#7113 = CARTESIAN_POINT ( 'NONE',  ( 1.937849085826861328, 10.00000000000000000, 1.000000000000000000 ) ) ;
#7114 = CARTESIAN_POINT ( 'NONE',  ( 10.37844141768317741, -24.50000000000000000, 3.449312527122335048 ) ) ;
#7115 = CARTESIAN_POINT ( 'NONE',  ( -12.64751377014909828, -19.11305460747000495, 5.510446717915143289 ) ) ;
#7116 = CARTESIAN_POINT ( 'NONE',  ( -4.847191417683177406, -20.91377862118959285, 1.020995438708345082 ) ) ;
#7117 = ORIENTED_EDGE ( 'NONE', *, *, #14786, .F. ) ;
#7118 = CARTESIAN_POINT ( 'NONE',  ( 1.811130159782011528, 4.999999999999999112, 1.000000000000000000 ) ) ;
#7119 = CARTESIAN_POINT ( 'NONE',  ( 0.6250000000000005551, 0.000000000000000000, 1.000000000000000000 ) ) ;
#7120 = CARTESIAN_POINT ( 'NONE',  ( -13.85593616229004610, 4.037276195647738319, 5.992122970672676630 ) ) ;
#7121 = VECTOR ( 'NONE', #9003, 1000.000000000000000 ) ;
#7122 = CARTESIAN_POINT ( 'NONE',  ( 11.40280858231679595, -22.46490103525074034, 2.520995438708341307 ) ) ;
#7123 = EDGE_CURVE ( 'NONE', #12057, #18833, #3063, .T. ) ;
#7124 = DIRECTION ( 'NONE',  ( 0.000000000000000000, -1.000000000000000000, 0.000000000000000000 ) ) ;
#7125 = ORIENTED_EDGE ( 'NONE', *, *, #1030, .T. ) ;
#7126 = ADVANCED_FACE ( 'NONE', ( #18962 ), #11309, .F. ) ;
#7127 = VERTEX_POINT ( 'NONE', #8082 ) ;
#7128 = CARTESIAN_POINT ( 'NONE',  ( 13.66279757975024722, -5.716222222589476765, 5.784013032957989964 ) ) ;
#7129 = LINE ( 'NONE', #13492, #16778 ) ;
#7130 = FILL_AREA_STYLE ('',( #3978 ) ) ;
#7131 = ORIENTED_EDGE ( 'NONE', *, *, #12824, .F. ) ;
#7132 = CARTESIAN_POINT ( 'NONE',  ( 0.6250000000000005551, 16.00000000000000000, 1.000000000000000000 ) ) ;
#7133 = CARTESIAN_POINT ( 'NONE',  ( 0.000000000000000000, 10.00000000000000000, 1.000000000000000000 ) ) ;
#7134 = CYLINDRICAL_SURFACE ( 'NONE', #16319, 10.00000000000000000 ) ;
#7135 = CARTESIAN_POINT ( 'NONE',  ( 13.47096266223369376, -15.40388555723029462, 5.575679699623145247 ) ) ;
#7136 = FACE_OUTER_BOUND ( 'NONE', #20465, .T. ) ;
#7137 = CARTESIAN_POINT ( 'NONE',  ( 0.9854920305337622199, -8.364917468222230923, 2.372643865078341019 ) ) ;
#7138 = EDGE_CURVE ( 'NONE', #2445, #2409, #4726, .T. ) ;
#7139 = CARTESIAN_POINT ( 'NONE',  ( 11.00000000000000000, -23.83493649053891517, 4.999999999999999112 ) ) ;
#7140 = CARTESIAN_POINT ( 'NONE',  ( -13.12526104302547836, 5.013182672784613381, 5.066812735559260261 ) ) ;
#7141 = LINE ( 'NONE', #12624, #13860 ) ;
#7142 = CARTESIAN_POINT ( 'NONE',  ( 12.34030858231679240, -22.67418626127525982, 5.270995438708342640 ) ) ;
#7143 = CARTESIAN_POINT ( 'NONE',  ( -13.44712222274167246, -17.35782775154002522, 6.283692769197384287 ) ) ;
#7144 = FACE_OUTER_BOUND ( 'NONE', #3212, .T. ) ;
#7145 = CARTESIAN_POINT ( 'NONE',  ( 7.465308582316796837, -20.97900456129165647, 3.863526089495444626 ) ) ;
#7146 = CARTESIAN_POINT ( 'NONE',  ( 6.534691417683176518, -20.22900456129164581, 2.825813738724747726 ) ) ;
#7147 = CARTESIAN_POINT ( 'NONE',  ( -9.902808582316794173, -22.77556120703056308, 1.770995438708339975 ) ) ;
#7148 = VECTOR ( 'NONE', #1998, 1000.000000000000000 ) ;
#7149 = EDGE_LOOP ( 'NONE', ( #9718, #19248, #15719, #5595, #14497, #4825 ) ) ;
#7150 = CARTESIAN_POINT ( 'NONE',  ( 13.08107971211413378, 2.032025461757085427, 6.715204579155630960 ) ) ;
#7151 = CARTESIAN_POINT ( 'NONE',  ( 13.09455366754861139, 4.212460211200554916, 5.160171780694988719 ) ) ;
#7152 = DIRECTION ( 'NONE',  ( 0.000000000000000000, 1.000000000000000000, 0.000000000000000000 ) ) ;
#7153 = VERTEX_POINT ( 'NONE', #17694 ) ;
#7154 = EDGE_LOOP ( 'NONE', ( #5230, #17777, #3541, #7748 ) ) ;
#7155 = LINE ( 'NONE', #14783, #18803 ) ;
#7156 = FACE_OUTER_BOUND ( 'NONE', #8056, .T. ) ;
#7157 = DIRECTION ( 'NONE',  ( -0.000000000000000000, -0.8660254037844363761, 0.5000000000000041078 ) ) ;
#7158 = CARTESIAN_POINT ( 'NONE',  ( 0.000000000000000000, 10.00000000000000000, 1.000000000000000000 ) ) ;
#7159 = CARTESIAN_POINT ( 'NONE',  ( 1.619022621591186928, -9.864917468222230923, 2.372643865078341019 ) ) ;
#7160 = PLANE ( 'NONE',  #4682 ) ;
#7161 = CARTESIAN_POINT ( 'NONE',  ( 2.687849085826861995, 10.00000000000000000, 1.000000000000000000 ) ) ;
#7162 = EDGE_CURVE ( 'NONE', #4975, #4594, #1488, .T. ) ;
#7163 = CARTESIAN_POINT ( 'NONE',  ( 12.67201297282924344, -20.43364036046235555, 3.544560889254710023 ) ) ;
#7164 = DIRECTION ( 'NONE',  ( -1.000000000000000000, 6.938893903907222067E-15, 0.000000000000000000 ) ) ;
#7165 = CARTESIAN_POINT ( 'NONE',  ( -9.809058582316794173, -23.27327832286945153, 2.298404588716537411 ) ) ;
#7166 = CARTESIAN_POINT ( 'NONE',  ( -4.181771508648414404, -14.78356139460145968, 3.271079850667843125 ) ) ;
#7167 = ORIENTED_EDGE ( 'NONE', *, *, #11460, .T. ) ;
#7168 = CARTESIAN_POINT ( 'NONE',  ( -13.37499999998404299, -19.49999999996810729, 2.793053905886972998 ) ) ;
#7169 = CARTESIAN_POINT ( 'NONE',  ( -7.277808582316794173, -20.27099543870833642, 2.724438792969431589 ) ) ;
#7170 = CARTESIAN_POINT ( 'NONE',  ( 12.34030858231679773, -22.98484643305508612, 6.020995438708344416 ) ) ;
#7171 = CARTESIAN_POINT ( 'NONE',  ( -8.878441417683177406, -22.99999999999999645, 3.449312527122335048 ) ) ;
#7172 = ORIENTED_EDGE ( 'NONE', *, *, #7601, .T. ) ;
#7173 = CARTESIAN_POINT ( 'NONE',  ( 13.37883250981221472, -20.05645825448334563, 5.102688967256983510 ) ) ;
#7174 = DIRECTION ( 'NONE',  ( 0.000000000000000000, -0.000000000000000000, -1.000000000000000000 ) ) ;
#7175 = ORIENTED_EDGE ( 'NONE', *, *, #3747, .F. ) ;
#7176 = ORIENTED_EDGE ( 'NONE', *, *, #10552, .T. ) ;
#7177 = CARTESIAN_POINT ( 'NONE',  ( 17.80017143803810242, 0.000000000000000000, 1.000000000000000000 ) ) ;
#7178 = VERTEX_POINT ( 'NONE', #3163 ) ;
#7179 = CARTESIAN_POINT ( 'NONE',  ( -13.37499999999998224, -20.25000000000006395, 4.416666666666681174 ) ) ;
#7180 = VERTEX_POINT ( 'NONE', #12663 ) ;
#7181 = FACE_OUTER_BOUND ( 'NONE', #19276, .T. ) ;
#7182 = DIRECTION ( 'NONE',  ( -0.000000000000000000, -0.000000000000000000, -1.000000000000000000 ) ) ;
#7183 = VECTOR ( 'NONE', #14262, 1000.000000000000000 ) ;
#7184 = DIRECTION ( 'NONE',  ( -0.000000000000000000, 0.000000000000000000, 1.000000000000000000 ) ) ;
#7185 = CARTESIAN_POINT ( 'NONE',  ( 3.951988298270009636, -13.15210598010094323, 2.852089508627633219 ) ) ;
#7186 = CARTESIAN_POINT ( 'NONE',  ( -6.621558582316794173, -23.74999999999999645, 3.550687472877651629 ) ) ;
#7187 = ADVANCED_FACE ( 'NONE', ( #9330 ), #9535, .T. ) ;
#7188 = CARTESIAN_POINT ( 'NONE',  ( 13.86796007304617717, 3.894483688830428836, 6.740724019197413597 ) ) ;
#7189 = DIRECTION ( 'NONE',  ( -1.000000000000000000, 0.000000000000000000, 0.000000000000000000 ) ) ;
#7190 = CARTESIAN_POINT ( 'NONE',  ( 11.12844141768317741, -20.99999999999999645, 3.550687472877664952 ) ) ;
#7191 = LINE ( 'NONE', #13765, #523 ) ;
#7192 = CARTESIAN_POINT ( 'NONE',  ( -3.974842109207560537, -21.92432777746334693, 4.506404853634142782 ) ) ;
#7193 = CARTESIAN_POINT ( 'NONE',  ( -10.19094141768317741, -23.80360840875937001, 5.231925497173365081 ) ) ;
#7194 = ORIENTED_EDGE ( 'NONE', *, *, #16202, .T. ) ;
#7195 = ADVANCED_FACE ( 'NONE', ( #17484 ), #5037, .T. ) ;
#7196 = CARTESIAN_POINT ( 'NONE',  ( 12.62500004114794372, -19.49999792202770621, 4.520295319612473328 ) ) ;
#7197 = CARTESIAN_POINT ( 'NONE',  ( -13.12529397354238192, 5.014845663890295846, 4.333333333333382775 ) ) ;
#7198 = EDGE_LOOP ( 'NONE', ( #9744, #18158, #4922, #15804 ) ) ;
#7199 = EDGE_CURVE ( 'NONE', #4996, #20631, #2950, .T. ) ;
#7200 = CARTESIAN_POINT ( 'NONE',  ( -9.805650798910056309, 9.000000000000001776, 1.000000000000000000 ) ) ;
#7201 = CARTESIAN_POINT ( 'NONE',  ( 0.000000000000000000, 4.999999999999999112, 1.000000000000000000 ) ) ;
#7202 = VERTEX_POINT ( 'NONE', #19176 ) ;
#7203 = ORIENTED_EDGE ( 'NONE', *, *, #16803, .T. ) ;
#7204 = AXIS2_PLACEMENT_3D ( 'NONE', #12735, #15564, #3023 ) ;
#7205 = ORIENTED_EDGE ( 'NONE', *, *, #15555, .T. ) ;
#7206 = DIRECTION ( 'NONE',  ( 1.040834085586084454E-15, 1.000000000000000000, 0.000000000000000000 ) ) ;
#7207 = LINE ( 'NONE', #20078, #14278 ) ;
#7208 = CARTESIAN_POINT ( 'NONE',  ( -1.652577328807104839, -9.114908150887895744, 1.622641472200749835 ) ) ;
#7209 = LINE ( 'NONE', #10454, #11697 ) ;
#7210 = DIRECTION ( 'NONE',  ( 0.000000000000000000, -1.000000000000000000, 0.000000000000000000 ) ) ;
#7211 = ADVANCED_FACE ( 'NONE', ( #12563 ), #15706, .F. ) ;
#7212 = PLANE ( 'NONE',  #3016 ) ;
#7213 = CARTESIAN_POINT ( 'NONE',  ( 11.69094141768317741, -23.80360840875937001, 5.231925497173365081 ) ) ;
#7214 = CARTESIAN_POINT ( 'NONE',  ( -12.64931222250080545, -19.02223276370786209, 5.512399842915133519 ) ) ;
#7215 = CARTESIAN_POINT ( 'NONE',  ( -9.534691417683177406, -19.47900456129164581, 2.515153566944927199 ) ) ;
#7216 = VERTEX_POINT ( 'NONE', #11008 ) ;
#7217 = CARTESIAN_POINT ( 'NONE',  ( 10.46530858231679417, -20.22900456129164937, 4.174186261275266929 ) ) ;
#7218 = LINE ( 'NONE', #1046, #8420 ) ;
#7219 = CARTESIAN_POINT ( 'NONE',  ( -13.37923893525309715, -20.78593376972237650, 5.366589449429977954 ) ) ;
#7220 = CARTESIAN_POINT ( 'NONE',  ( 13.09030858231679417, -21.32581373872472597, 1.729004561291657582 ) ) ;
#7221 = DIRECTION ( 'NONE',  ( -0.000000000000000000, -0.000000000000000000, -1.000000000000000000 ) ) ;
#7222 = EDGE_LOOP ( 'NONE', ( #1973, #504, #2555, #3560 ) ) ;
#7223 = ORIENTED_EDGE ( 'NONE', *, *, #1872, .F. ) ;
#7224 = CARTESIAN_POINT ( 'NONE',  ( 13.84983662433050178, 3.729249528687784920, 5.987138032956566214 ) ) ;
#7225 = LINE ( 'NONE', #19989, #12589 ) ;
#7226 = ORIENTED_EDGE ( 'NONE', *, *, #8211, .F. ) ;
#7227 = DIRECTION ( 'NONE',  ( 1.000000000000000000, 0.000000000000000000, -0.000000000000000000 ) ) ;
#7228 = VECTOR ( 'NONE', #13799, 1000.000000000000000 ) ;
#7229 = FACE_OUTER_BOUND ( 'NONE', #1196, .T. ) ;
#7230 = CARTESIAN_POINT ( 'NONE',  ( 9.555650798910054533, 4.999999999999999112, 1.000000000000000000 ) ) ;
#7231 = CYLINDRICAL_SURFACE ( 'NONE', #9256, 1.499999999999999556 ) ;
#7232 = FACE_OUTER_BOUND ( 'NONE', #19296, .T. ) ;
#7233 = CARTESIAN_POINT ( 'NONE',  ( 1.824488249492779879, -9.124319963227819130, 2.375058613629473570 ) ) ;
#7234 = EDGE_CURVE ( 'NONE', #17871, #16350, #9437, .T. ) ;
#7235 = EDGE_CURVE ( 'NONE', #18752, #13489, #13233, .T. ) ;
#7236 = DIRECTION ( 'NONE',  ( 1.000000000000000000, 0.000000000000000000, 0.000000000000000000 ) ) ;
#7237 = CARTESIAN_POINT ( 'NONE',  ( -12.62691554569741648, -19.40326494227377907, 4.703927990036796736 ) ) ;
#7238 =( NAMED_UNIT ( * ) SI_UNIT ( $, .STERADIAN. ) SOLID_ANGLE_UNIT ( ) );
#7239 = CARTESIAN_POINT ( 'NONE',  ( 12.80905858231679417, -23.27327832286945153, 2.298404588716537411 ) ) ;
#7240 = CARTESIAN_POINT ( 'NONE',  ( -13.37499999999998401, -20.99999999999999645, 3.146526952850934755 ) ) ;
#7241 = EDGE_CURVE ( 'NONE', #19, #9082, #1586, .T. ) ;
#7242 = DIRECTION ( 'NONE',  ( -5.204170427930411817E-15, 1.000000000000000000, 0.000000000000000000 ) ) ;
#7243 = CARTESIAN_POINT ( 'NONE',  ( 11.21530858231679417, -23.77099543870833998, 2.825813738724734847 ) ) ;
#7244 = CARTESIAN_POINT ( 'NONE',  ( 9.065941417683177406, -22.67126532539353789, 2.757051763020445634 ) ) ;
#7245 = CARTESIAN_POINT ( 'NONE',  ( -4.746558582316795061, -21.94931252712234127, 4.499999999999999112 ) ) ;
#7246 = VERTEX_POINT ( 'NONE', #7023 ) ;
#7247 = CARTESIAN_POINT ( 'NONE',  ( 12.85087781109329974, -9.593170539812428288, 6.465204579154565145 ) ) ;
#7248 = CARTESIAN_POINT ( 'NONE',  ( 12.62499999999998224, -19.50000000000006040, 4.416666666666682062 ) ) ;
#7249 = DIRECTION ( 'NONE',  ( 0.000000000000000000, -1.000000000000000000, 0.000000000000000000 ) ) ;
#7250 = VERTEX_POINT ( 'NONE', #18213 ) ;
#7251 = EDGE_CURVE ( 'NONE', #10835, #17227, #13389, .T. ) ;
#7252 = ORIENTED_EDGE ( 'NONE', *, *, #2362, .T. ) ;
#7253 = DIRECTION ( 'NONE',  ( -1.000000000000000000, 0.000000000000000000, 0.000000000000000000 ) ) ;
#7254 = AXIS2_PLACEMENT_3D ( 'NONE', #15769, #1349, #6058 ) ;
#7255 = DIRECTION ( 'NONE',  ( 0.000000000000000000, 1.000000000000000000, -0.000000000000000000 ) ) ;
#7256 = LINE ( 'NONE', #8829, #7966 ) ;
#7257 = DIRECTION ( 'NONE',  ( 0.000000000000000000, 1.000000000000000000, -0.000000000000000000 ) ) ;
#7258 = CARTESIAN_POINT ( 'NONE',  ( 2.659620708751979645, -10.38426118526329489, 2.698636689302993830 ) ) ;
#7259 = CARTESIAN_POINT ( 'NONE',  ( -20.92243175760212637, 4.999999999999999112, 1.000000000000000000 ) ) ;
#7260 = VECTOR ( 'NONE', #19281, 1000.000000000000114 ) ;
#7261 = CARTESIAN_POINT ( 'NONE',  ( -21.42243175760212637, 0.000000000000000000, 1.000000000000000000 ) ) ;
#7262 = CARTESIAN_POINT ( 'NONE',  ( 30.00000000000000000, 3.000000000000000000, 1.000000000000000000 ) ) ;
#7263 = CARTESIAN_POINT ( 'NONE',  ( -11.87155858231679595, -19.49999999999998934, 3.449312527122348371 ) ) ;
#7264 = CARTESIAN_POINT ( 'NONE',  ( -1.754777266914451461, -9.116337928146160507, 1.623008667563337726 ) ) ;
#7265 = EDGE_LOOP ( 'NONE', ( #10359, #4771, #4584, #3801 ) ) ;
#7266 = VECTOR ( 'NONE', #19148, 1000.000000000000227 ) ;
#7267 = CARTESIAN_POINT ( 'NONE',  ( -13.37939227869017600, -19.27818992614120575, 4.741950614318236390 ) ) ;
#7268 = CARTESIAN_POINT ( 'NONE',  ( -9.996558582316794173, -22.05068747287764452, 1.749999999999998446 ) ) ;
#7269 = CARTESIAN_POINT ( 'NONE',  ( 10.56594141768317741, -23.73192549717336064, 1.696391591240623331 ) ) ;
#7270 = CARTESIAN_POINT ( 'NONE',  ( -11.78469141768317741, -23.02099543870834353, 3.863526089495429972 ) ) ;
#7271 = ORIENTED_EDGE ( 'NONE', *, *, #19739, .F. ) ;
#7272 = CARTESIAN_POINT ( 'NONE',  ( 13.77789853026076550, 0.09637577819625635367, 5.909013032956687006 ) ) ;
#7273 = CARTESIAN_POINT ( 'NONE',  ( -4.250698171653726654, 0.000000000000000000, 1.000000000000000000 ) ) ;
#7274 = EDGE_LOOP ( 'NONE', ( #3819, #19124, #2720, #13936 ) ) ;
#7275 = ORIENTED_EDGE ( 'NONE', *, *, #2171, .T. ) ;
#7276 = EDGE_CURVE ( 'NONE', #17965, #11896, #6716, .T. ) ;
#7277 = DIRECTION ( 'NONE',  ( 0.000000000000000000, -1.000000000000000000, 0.000000000000000000 ) ) ;
#7278 = ORIENTED_EDGE ( 'NONE', *, *, #18139, .T. ) ;
#7279 = LINE ( 'NONE', #486, #6435 ) ;
#7280 = ORIENTED_EDGE ( 'NONE', *, *, #661, .F. ) ;
#7281 = PLANE ( 'NONE',  #4320 ) ;
#7282 = CARTESIAN_POINT ( 'NONE',  ( 8.119520639128047890, 9.000000000000001776, 1.000000000000000000 ) ) ;
#7283 = CARTESIAN_POINT ( 'NONE',  ( -17.05017143803810242, 0.000000000000000000, 1.000000000000000000 ) ) ;
#7284 = CARTESIAN_POINT ( 'NONE',  ( 2.076833265075072266, -8.407161531158021006, 2.383492984350220389 ) ) ;
#7285 = DIRECTION ( 'NONE',  ( 1.000000000000000000, -0.000000000000000000, 0.000000000000000000 ) ) ;
#7286 = CARTESIAN_POINT ( 'NONE',  ( 12.62543384439201510, -20.97809085820452424, 4.782403934559678937 ) ) ;
#7287 = DIRECTION ( 'NONE',  ( -0.000000000000000000, -0.000000000000000000, -1.000000000000000000 ) ) ;
#7288 = CARTESIAN_POINT ( 'NONE',  ( 16.37779268661489596, 11.64110105645932691, 10.00000000000000000 ) ) ;
#7289 = CARTESIAN_POINT ( 'NONE',  ( 6.065941417683177406, -23.20159541128344927, 2.226721677130534705 ) ) ;
#7290 = DIRECTION ( 'NONE',  ( 0.000000000000000000, 0.000000000000000000, -1.000000000000000000 ) ) ;
#7291 = CARTESIAN_POINT ( 'NONE',  ( -6.065941417683177406, -22.67126532539353789, 2.757051763020445634 ) ) ;
#7292 = CARTESIAN_POINT ( 'NONE',  ( -10.00344141768317741, -22.05068747287766229, 6.000000000000001776 ) ) ;
#7293 = AXIS2_PLACEMENT_3D ( 'NONE', #5506, #10215, #3628 ) ;
#7294 = EDGE_LOOP ( 'NONE', ( #435, #14277, #5063, #3086 ) ) ;
#7295 = CARTESIAN_POINT ( 'NONE',  ( 13.12529380813666435, 5.014837310896125722, 5.033295791462342628 ) ) ;
#7296 = CARTESIAN_POINT ( 'NONE',  ( -13.05696142222617695, 1.564051822406025583, 5.955108176248398166 ) ) ;
#7297 = ORIENTED_EDGE ( 'NONE', *, *, #12365, .T. ) ;
#7298 = CIRCLE ( 'NONE', #9632, 10.00000000000000000 ) ;
#7299 = CARTESIAN_POINT ( 'NONE',  ( -1.437849085826860884, 10.00000000000000000, 1.000000000000000000 ) ) ;
#7300 = CARTESIAN_POINT ( 'NONE',  ( 27.94203811574921659, 9.999999999999998224, 1.000000000000000000 ) ) ;
#7301 = ORIENTED_EDGE ( 'NONE', *, *, #20162, .T. ) ;
#7302 = VERTEX_POINT ( 'NONE', #634 ) ;
#7303 = EDGE_CURVE ( 'NONE', #10724, #6116, #3104, .T. ) ;
#7304 = ORIENTED_EDGE ( 'NONE', *, *, #9518, .T. ) ;
#7305 = FACE_OUTER_BOUND ( 'NONE', #17999, .T. ) ;
#7306 = PLANE ( 'NONE',  #18672 ) ;
#7307 = VECTOR ( 'NONE', #848, 1000.000000000000000 ) ;
#7308 = ADVANCED_FACE ( 'NONE', ( #8489 ), #11613, .T. ) ;
#7309 = CARTESIAN_POINT ( 'NONE',  ( -2.506848361495492394, -9.459347215042898327, 1.711100304737409150 ) ) ;
#7310 = LINE ( 'NONE', #16920, #4638 ) ;
#7311 = CARTESIAN_POINT ( 'NONE',  ( -8.376396343307449754, 16.00000000000000000, 1.000000000000000000 ) ) ;
#7312 = EDGE_CURVE ( 'NONE', #13849, #20560, #18115, .T. ) ;
#7313 = VECTOR ( 'NONE', #19970, 1000.000000000000000 ) ;
#7314 = CARTESIAN_POINT ( 'NONE',  ( 11.00000000000000000, -20.29006350946107418, 5.466506350946110260 ) ) ;
#7315 = CARTESIAN_POINT ( 'NONE',  ( 10.56594141768317741, -23.73192549717336064, 1.696391591240623331 ) ) ;
#7316 = CARTESIAN_POINT ( 'NONE',  ( -12.62599079447150885, -20.19996487918709249, 4.820256282269618886 ) ) ;
#7317 = CARTESIAN_POINT ( 'NONE',  ( -6.909691417683176518, -21.01515356694492098, 6.020995438708349745 ) ) ;
#7318 = ORIENTED_EDGE ( 'NONE', *, *, #5673, .F. ) ;
#7319 = CARTESIAN_POINT ( 'NONE',  ( 12.05905858231679417, -20.72672167713054137, 4.701595411283463477 ) ) ;
#7320 = DIRECTION ( 'NONE',  ( 0.000000000000000000, 0.000000000000000000, 1.000000000000000000 ) ) ;
#7321 = CARTESIAN_POINT ( 'NONE',  ( -13.90258797164900884, 5.643192568275169130, 5.568788873356017355 ) ) ;
#7322 = AXIS2_PLACEMENT_3D ( 'NONE', #8419, #2229, #8614 ) ;
#7323 = CARTESIAN_POINT ( 'NONE',  ( 11.68405858231679417, -20.79840458871652942, 2.226721677130544030 ) ) ;
#7324 = CARTESIAN_POINT ( 'NONE',  ( -10.43924542913431175, 11.64110105645932691, 0.000000000000000000 ) ) ;
#7325 = AXIS2_PLACEMENT_3D ( 'NONE', #1051, #7743, #9409 ) ;
#7326 = VERTEX_POINT ( 'NONE', #8279 ) ;
#7327 = EDGE_LOOP ( 'NONE', ( #9205, #5739, #9968, #6931 ) ) ;
#7328 = CARTESIAN_POINT ( 'NONE',  ( 13.87470602645761986, 4.985154336109792972, 4.833333333333344584 ) ) ;
#7329 = CARTESIAN_POINT ( 'NONE',  ( -20.00000000000000000, 2.499999999999999556, 2.000000000000000000 ) ) ;
#7330 = VERTEX_POINT ( 'NONE', #16328 ) ;
#7331 = EDGE_CURVE ( 'NONE', #20224, #5681, #8586, .T. ) ;
#7332 = DIRECTION ( 'NONE',  ( -1.000000000000000000, 0.000000000000000000, 0.000000000000000000 ) ) ;
#7333 = LINE ( 'NONE', #18116, #5023 ) ;
#7334 = CARTESIAN_POINT ( 'NONE',  ( -11.49655858231679417, -22.05068747287764452, 1.749999999999998446 ) ) ;
#7335 = CARTESIAN_POINT ( 'NONE',  ( 13.87470602645761986, 4.985154336109792972, 4.666666666666619889 ) ) ;
#7336 = VECTOR ( 'NONE', #14603, 1000.000000000000000 ) ;
#7337 = VECTOR ( 'NONE', #18895, 1000.000000000000000 ) ;
#7338 = DIRECTION ( 'NONE',  ( -6.938893903907232322E-16, 1.000000000000000000, 0.000000000000000000 ) ) ;
#7339 = CARTESIAN_POINT ( 'NONE',  ( 2.844469389063872811, -10.54053385813977606, 1.988770633557972012 ) ) ;
#7340 = APPLICATION_CONTEXT ( 'automotive_design' ) ;
#7341 = AXIS2_PLACEMENT_3D ( 'NONE', #13715, #16957, #9023 ) ;
#7342 = DIRECTION ( 'NONE',  ( 1.000000000000000000, 0.000000000000000000, -0.000000000000000000 ) ) ;
#7343 = CARTESIAN_POINT ( 'NONE',  ( -13.37503747255156306, -19.49810763614315690, 4.531249681074674740 ) ) ;
#7344 = CARTESIAN_POINT ( 'NONE',  ( 11.87155858231679417, -20.24999999999999289, 3.449312527122348371 ) ) ;
#7345 = CARTESIAN_POINT ( 'NONE',  ( -13.37499999999998401, -20.99999999999999645, 3.666666666666654084 ) ) ;
#7346 = EDGE_CURVE ( 'NONE', #15234, #3417, #9845, .T. ) ;
#7347 = CARTESIAN_POINT ( 'NONE',  ( 0.000000000000000000, 4.999999999999999112, 1.000000000000000000 ) ) ;
#7348 = CARTESIAN_POINT ( 'NONE',  ( 10.46530858231679417, -20.22900456129164937, 4.174186261275266929 ) ) ;
#7349 = CARTESIAN_POINT ( 'NONE',  ( 10.94094141768317741, -21.25705176302044208, 2.828734674606458555 ) ) ;
#7350 = CARTESIAN_POINT ( 'NONE',  ( -11.59030858231679417, -21.32581373872472597, 1.729004561291657582 ) ) ;
#7351 = ORIENTED_EDGE ( 'NONE', *, *, #6720, .T. ) ;
#7352 = CARTESIAN_POINT ( 'NONE',  ( 12.62500000000002132, -19.50000000000273559, 4.083333333315724012 ) ) ;
#7353 = CARTESIAN_POINT ( 'NONE',  ( 8.876396343307449754, 16.00000000000000000, 1.000000000000000000 ) ) ;
#7354 = ORIENTED_EDGE ( 'NONE', *, *, #20628, .F. ) ;
#7355 = EDGE_CURVE ( 'NONE', #5494, #1315, #3671, .T. ) ;
#7356 = ORIENTED_EDGE ( 'NONE', *, *, #14763, .T. ) ;
#7357 = EDGE_CURVE ( 'NONE', #8920, #11466, #6792, .T. ) ;
#7358 = CARTESIAN_POINT ( 'NONE',  ( -3.999999999999999112, -7.500000000000047073, 7.000000000000000000 ) ) ;
#7359 = CIRCLE ( 'NONE', #1006, 10.00000000000000000 ) ;
#7360 = VECTOR ( 'NONE', #13572, 1000.000000000000000 ) ;
#7361 = CARTESIAN_POINT ( 'NONE',  ( -12.66849571425264287, -18.05346643024382303, 5.533233176248494978 ) ) ;
#7362 = CARTESIAN_POINT ( 'NONE',  ( 15.00000000000000355, -5.999999999999996447, 1.000000000000000000 ) ) ;
#7363 = CARTESIAN_POINT ( 'NONE',  ( -13.66279757975024722, -5.716222222589476765, 5.784013032957989964 ) ) ;
#7364 = DIRECTION ( 'NONE',  ( 1.000000000000000000, -0.000000000000000000, 0.000000000000000000 ) ) ;
#7365 = CARTESIAN_POINT ( 'NONE',  ( 1.857501949683560971, -9.975525523312803955, 2.401050223243493154 ) ) ;
#7366 = FACE_OUTER_BOUND ( 'NONE', #2825, .T. ) ;
#7367 = DIRECTION ( 'NONE',  ( 0.000000000000000000, 1.000000000000000000, 0.000000000000000000 ) ) ;
#7368 = ADVANCED_FACE ( 'NONE', ( #19486 ), #10054, .T. ) ;
#7369 = DIRECTION ( 'NONE',  ( -0.000000000000000000, -0.000000000000000000, -1.000000000000000000 ) ) ;
#7370 = CARTESIAN_POINT ( 'NONE',  ( -8.684058582316795949, -20.26807450282662160, 1.696391591240633101 ) ) ;
#7371 = CARTESIAN_POINT ( 'NONE',  ( -2.340131407102140848, -12.21153219924485889, 2.225301406344140531 ) ) ;
#7372 = ORIENTED_EDGE ( 'NONE', *, *, #492, .T. ) ;
#7373 = CARTESIAN_POINT ( 'NONE',  ( -13.37930517931174634, -19.28258844475809042, 4.742233558278135419 ) ) ;
#7374 = VECTOR ( 'NONE', #17319, 1000.000000000000000 ) ;
#7375 = CARTESIAN_POINT ( 'NONE',  ( -2.061130159782011972, 4.999999999999999112, 0.000000000000000000 ) ) ;
#7376 = AXIS2_PLACEMENT_3D ( 'NONE', #12095, #18486, #12404 ) ;
#7377 = CARTESIAN_POINT ( 'NONE',  ( 6.246558582316795949, -21.94931252712234127, 6.000000000000001776 ) ) ;
#7378 = CARTESIAN_POINT ( 'NONE',  ( -10.19094141768317741, -22.74294823697955081, 4.171265325393542334 ) ) ;
#7379 = VERTEX_POINT ( 'NONE', #6911 ) ;
#7380 = CARTESIAN_POINT ( 'NONE',  ( 13.37500000000002132, -20.25000000000274269, 4.083333333315724012 ) ) ;
#7381 = CARTESIAN_POINT ( 'NONE',  ( -13.12500000000000178, 5.000000000000047962, 2.000000000000000000 ) ) ;
#7382 = VERTEX_POINT ( 'NONE', #7132 ) ;
#7383 = ORIENTED_EDGE ( 'NONE', *, *, #14739, .T. ) ;
#7384 = CARTESIAN_POINT ( 'NONE',  ( 4.999999999999998224, -7.500000000000047073, 9.999999999999998224 ) ) ;
#7385 = EDGE_CURVE ( 'NONE', #16591, #14054, #8692, .T. ) ;
#7386 = ORIENTED_EDGE ( 'NONE', *, *, #3038, .F. ) ;
#7387 = EDGE_CURVE ( 'NONE', #5651, #13228, #6814, .T. ) ;
#7388 = CARTESIAN_POINT ( 'NONE',  ( -13.85223456079946303, 3.850345320370711644, 5.989742199623227847 ) ) ;
#7389 = CIRCLE ( 'NONE', #14725, 10.00000000000000000 ) ;
#7390 = ORIENTED_EDGE ( 'NONE', *, *, #9739, .T. ) ;
#7391 = DIRECTION ( 'NONE',  ( 1.000000000000000000, 0.000000000000000000, -0.000000000000000000 ) ) ;
#7392 = CARTESIAN_POINT ( 'NONE',  ( 20.50349085826861995, 11.64110105645932691, 0.000000000000000000 ) ) ;
#7393 = AXIS2_PLACEMENT_3D ( 'NONE', #6733, #13100, #11533 ) ;
#7394 = AXIS2_PLACEMENT_3D ( 'NONE', #9642, #19182, #4836 ) ;
#7395 = CARTESIAN_POINT ( 'NONE',  ( -24.87918902992234393, 10.00000000000000000, 1.000000000000000000 ) ) ;
#7396 = CARTESIAN_POINT ( 'NONE',  ( 1.619022621591187150, -9.114917468222230923, 2.372643865078341019 ) ) ;
#7397 = CARTESIAN_POINT ( 'NONE',  ( -24.12918902992234393, 16.00000000000000000, 1.000000000000000000 ) ) ;
#7398 = EDGE_CURVE ( 'NONE', #15234, #6239, #15063, .T. ) ;
#7399 = CARTESIAN_POINT ( 'NONE',  ( 12.66024186180961308, -19.22028597861421417, 6.258173329156003106 ) ) ;
#7400 = CARTESIAN_POINT ( 'NONE',  ( -30.00000000000000000, 3.000000000000000000, 1.000000000000000000 ) ) ;
#7401 = CARTESIAN_POINT ( 'NONE',  ( -14.49999999999999645, -22.99999999999998579, 1.000000000000000000 ) ) ;
#7402 = CARTESIAN_POINT ( 'NONE',  ( -14.49999999999998579, -25.49999999999999645, 1.000000000000000000 ) ) ;
#7403 = CARTESIAN_POINT ( 'NONE',  ( 5.597191417683179182, -22.77556120703057729, 5.229004561291655584 ) ) ;
#7404 = CARTESIAN_POINT ( 'NONE',  ( -12.62524871736568954, -20.23743977303344010, 4.661898514667671023 ) ) ;
#7405 = CARTESIAN_POINT ( 'NONE',  ( -10.09030858231679595, -21.63647391050454871, 2.479004561291657804 ) ) ;
#7406 = CARTESIAN_POINT ( 'NONE',  ( -9.159691417683175629, -22.98484643305507191, 0.9790045612916508100 ) ) ;
#7407 = ORIENTED_EDGE ( 'NONE', *, *, #18376, .T. ) ;
#7408 = CARTESIAN_POINT ( 'NONE',  ( 12.82182472306881671, -9.560351485048736109, 4.965845106672846399 ) ) ;
#7409 = CARTESIAN_POINT ( 'NONE',  ( -13.11514659413808737, 4.502403003978772134, 5.887634658581065494 ) ) ;
#7410 = EDGE_LOOP ( 'NONE', ( #11492, #10050, #6906, #6144 ) ) ;
#7411 = AXIS2_PLACEMENT_3D ( 'NONE', #1905, #12990, #8288 ) ;
#7412 = LINE ( 'NONE', #7200, #10289 ) ;
#7413 = PLANE ( 'NONE',  #13666 ) ;
#7414 = ORIENTED_EDGE ( 'NONE', *, *, #6322, .T. ) ;
#7415 = CARTESIAN_POINT ( 'NONE',  ( 1.742625132518061504, -9.872369070458363538, 2.374557585393312298 ) ) ;
#7416 = VERTEX_POINT ( 'NONE', #14759 ) ;
#7417 = ORIENTED_EDGE ( 'NONE', *, *, #3262, .F. ) ;
#7418 = CARTESIAN_POINT ( 'NONE',  ( -9.305650798910056309, 4.999999999999999112, 1.000000000000000000 ) ) ;
#7419 = CARTESIAN_POINT ( 'NONE',  ( 0.000000000000000000, 9.000000000000001776, 1.000000000000000000 ) ) ;
#7420 = CARTESIAN_POINT ( 'NONE',  ( -1.709849555000590104, -9.864920124259167977, 1.622644547201689713 ) ) ;
#7421 = CARTESIAN_POINT ( 'NONE',  ( -9.000000000000000000, -9.999999999999992895, 2.500000000000000000 ) ) ;
#7422 = CARTESIAN_POINT ( 'NONE',  ( -0.1250000000000035805, 0.000000000000000000, 0.000000000000000000 ) ) ;
#7423 = CARTESIAN_POINT ( 'NONE',  ( -0.000000000000000000, 11.64110105645932691, 0.000000000000000000 ) ) ;
#7424 = CARTESIAN_POINT ( 'NONE',  ( 10.28469141768317741, -24.52099543870834708, 4.484846433055073689 ) ) ;
#7425 = CARTESIAN_POINT ( 'NONE',  ( -13.12463908936614132, 4.981774012991869505, 5.264611377988129171 ) ) ;
#7426 = CARTESIAN_POINT ( 'NONE',  ( -5.503441417683177406, -22.05068747287766229, 6.000000000000001776 ) ) ;
#7427 = EDGE_CURVE ( 'NONE', #15500, #13273, #11517, .T. ) ;
#7428 = EDGE_LOOP ( 'NONE', ( #17152, #4905, #10208, #5618 ) ) ;
#7429 = CARTESIAN_POINT ( 'NONE',  ( 10.27780858231679417, -20.27099543870833642, 2.724438792969431589 ) ) ;
#7430 = DIRECTION ( 'NONE',  ( -1.000000000000000000, -0.000000000000000000, -0.000000000000000000 ) ) ;
#7431 = CARTESIAN_POINT ( 'NONE',  ( -13.37526900345969771, -20.98641532528209908, 4.724331462949078464 ) ) ;
#7432 = CARTESIAN_POINT ( 'NONE',  ( 11.30905858231679417, -23.27327832286945153, 2.298404588716537411 ) ) ;
#7433 = CARTESIAN_POINT ( 'NONE',  ( -0.000000000000000000, 11.64110105645932691, 0.000000000000000000 ) ) ;
#7434 = ORIENTED_EDGE ( 'NONE', *, *, #6960, .F. ) ;
#7435 = ORIENTED_EDGE ( 'NONE', *, *, #7717, .T. ) ;
#7436 = CARTESIAN_POINT ( 'NONE',  ( 13.37499999999998224, -20.99999999999991829, 4.333333333333343695 ) ) ;
#7437 = DIRECTION ( 'NONE',  ( -0.000000000000000000, 0.000000000000000000, -1.000000000000000000 ) ) ;
#7438 = VERTEX_POINT ( 'NONE', #11416 ) ;
#7439 = AXIS2_PLACEMENT_3D ( 'NONE', #11146, #3097, #8115 ) ;
#7440 = CARTESIAN_POINT ( 'NONE',  ( 0.000000000000000000, 10.00000000000000000, 1.000000000000000000 ) ) ;
#7441 = VERTEX_POINT ( 'NONE', #3566 ) ;
#7442 = CARTESIAN_POINT ( 'NONE',  ( -10.93405858231679417, -23.20159541128345992, 4.773278322869455970 ) ) ;
#7443 = LINE ( 'NONE', #6080, #235 ) ;
#7444 = DIRECTION ( 'NONE',  ( 0.000000000000000000, 0.000000000000000000, 1.000000000000000000 ) ) ;
#7445 = CARTESIAN_POINT ( 'NONE',  ( 2.506848361495492394, -9.459347215042898327, 1.711100304737409150 ) ) ;
#7446 = CARTESIAN_POINT ( 'NONE',  ( 0.000000000000000000, 9.000000000000001776, 0.000000000000000000 ) ) ;
#7447 = CARTESIAN_POINT ( 'NONE',  ( -13.09106898171683930, 4.036483576700608644, 5.256123545019964816 ) ) ;
#7448 = PLANE ( 'NONE',  #3073 ) ;
#7449 = CARTESIAN_POINT ( 'NONE',  ( -13.37671366598624800, -20.91345986769124465, 5.053911344471881506 ) ) ;
#7450 = AXIS2_PLACEMENT_3D ( 'NONE', #559, #6937, #7253 ) ;
#7451 = EDGE_CURVE ( 'NONE', #20560, #551, #9946, .T. ) ;
#7452 = CYLINDRICAL_SURFACE ( 'NONE', #13699, 10.00000000000000000 ) ;
#7453 = CARTESIAN_POINT ( 'NONE',  ( 11.12155858231679417, -23.74999999999999645, 3.550687472877651629 ) ) ;
#7454 = CARTESIAN_POINT ( 'NONE',  ( 10.65969141768317741, -22.36352608949543352, 2.479004561291652031 ) ) ;
#7455 = CARTESIAN_POINT ( 'NONE',  ( -11.77780858231679417, -20.27099543870833642, 2.724438792969431589 ) ) ;
#7456 = VERTEX_POINT ( 'NONE', #5344 ) ;
#7457 = EDGE_CURVE ( 'NONE', #16862, #4975, #10156, .T. ) ;
#7458 = CARTESIAN_POINT ( 'NONE',  ( 13.40368151590352497, -18.05158344687463412, 4.768708296715732153 ) ) ;
#7459 = EDGE_CURVE ( 'NONE', #7178, #8633, #5458, .T. ) ;
#7460 = CARTESIAN_POINT ( 'NONE',  ( 0.000000000000000000, 10.00000000000000000, 1.000000000000000000 ) ) ;
#7461 = ORIENTED_EDGE ( 'NONE', *, *, #19077, .F. ) ;
#7462 = VERTEX_POINT ( 'NONE', #5551 ) ;
#7463 = CARTESIAN_POINT ( 'NONE',  ( -14.49999999999999645, -22.99999999999998579, 4.000000000000000000 ) ) ;
#7464 = VECTOR ( 'NONE', #15884, 1000.000000000000000 ) ;
#7465 = CARTESIAN_POINT ( 'NONE',  ( -12.62500000000001954, -20.25000000000274269, 4.083333333315724012 ) ) ;
#7466 = CARTESIAN_POINT ( 'NONE',  ( -2.594671182134835163, -9.923034775318452461, 2.580184533305832861 ) ) ;
#7467 = CARTESIAN_POINT ( 'NONE',  ( -13.54769662923970763, -11.52882022337116119, 5.659013032956382361 ) ) ;
#7468 = DIRECTION ( 'NONE',  ( 0.000000000000000000, 0.1264857625231113059, 0.9919684228235025047 ) ) ;
#7469 = CARTESIAN_POINT ( 'NONE',  ( -12.62499999999998401, -20.24999999999998934, 2.439580858552613751 ) ) ;
#7470 = CARTESIAN_POINT ( 'NONE',  ( 11.00000000000000000, -20.16506350946107418, 5.000000000000000000 ) ) ;
#7471 = DIRECTION ( 'NONE',  ( -1.000000000000000000, 0.000000000000000000, 0.000000000000000000 ) ) ;
#7472 = EDGE_CURVE ( 'NONE', #6152, #11135, #846, .T. ) ;
#7473 = CARTESIAN_POINT ( 'NONE',  ( 4.687312169500630787, -21.49117650933202128, 5.277475135490085734 ) ) ;
#7474 = CARTESIAN_POINT ( 'NONE',  ( -12.34030858231679773, -22.98484643305508612, 6.020995438708344416 ) ) ;
#7475 = CARTESIAN_POINT ( 'NONE',  ( -2.830107938415192148, -10.43856789473369950, 1.962583737180462418 ) ) ;
#7476 = VERTEX_POINT ( 'NONE', #15478 ) ;
#7477 = CARTESIAN_POINT ( 'NONE',  ( -13.37499999999998224, -20.24999999999998934, 4.291666666666698937 ) ) ;
#7478 = CARTESIAN_POINT ( 'NONE',  ( 27.94203811574921303, 11.64110105645932691, 10.00000000000000000 ) ) ;
#7479 = CARTESIAN_POINT ( 'NONE',  ( 5.402808582316795949, -23.08622137881038938, 1.020995438708339309 ) ) ;
#7480 = CARTESIAN_POINT ( 'NONE',  ( -11.12844141768317741, -20.99999999999999645, 3.550687472877664952 ) ) ;
#7481 = ORIENTED_EDGE ( 'NONE', *, *, #7939, .T. ) ;
#7482 = CARTESIAN_POINT ( 'NONE',  ( 13.37500000000002132, -20.99999999999450395, 3.833333333368183382 ) ) ;
#7483 = DIRECTION ( 'NONE',  ( -0.000000000000000000, 0.000000000000000000, -1.000000000000000000 ) ) ;
#7484 = ORIENTED_EDGE ( 'NONE', *, *, #15015, .T. ) ;
#7485 = ORIENTED_EDGE ( 'NONE', *, *, #7649, .F. ) ;
#7486 = CARTESIAN_POINT ( 'NONE',  ( -20.00000000000000000, 0.000000000000000000, 1.000000000000000000 ) ) ;
#7487 = EDGE_LOOP ( 'NONE', ( #7914, #16075 ) ) ;
#7488 = CARTESIAN_POINT ( 'NONE',  ( -13.70116456325478893, -3.778689555664588973, 5.825679699621801433 ) ) ;
#7489 = AXIS2_PLACEMENT_3D ( 'NONE', #5998, #4118, #18554 ) ;
#7490 = EDGE_CURVE ( 'NONE', #7216, #12080, #10675, .T. ) ;
#7491 = CARTESIAN_POINT ( 'NONE',  ( 1.743623630681728542, -9.116095536440919744, 2.372946416531167557 ) ) ;
#7492 = ORIENTED_EDGE ( 'NONE', *, *, #19595, .T. ) ;
#7493 = CARTESIAN_POINT ( 'NONE',  ( 10.93924542913430820, 0.000000000000000000, 1.000000000000000000 ) ) ;
#7494 = DIRECTION ( 'NONE',  ( 1.000000000000000000, 0.000000000000000000, -0.000000000000000000 ) ) ;
#7495 = DIRECTION ( 'NONE',  ( 0.000000000000000000, -1.000000000000000000, 0.000000000000000000 ) ) ;
#7496 = CARTESIAN_POINT ( 'NONE',  ( 2.808565762442263303, -10.28561894962424716, 1.923303392614186924 ) ) ;
#7497 = DIRECTION ( 'NONE',  ( 0.000000000000000000, 1.000000000000000000, -0.000000000000000000 ) ) ;
#7498 = DIRECTION ( 'NONE',  ( 1.000000000000000000, 0.000000000000000000, 0.000000000000000000 ) ) ;
#7499 = ADVANCED_FACE ( 'NONE', ( #1058 ), #2831, .F. ) ;
#7500 = LINE ( 'NONE', #20368, #10321 ) ;
#7501 = DIRECTION ( 'NONE',  ( 5.204170427930411817E-15, -1.000000000000000000, 0.000000000000000000 ) ) ;
#7502 = EDGE_CURVE ( 'NONE', #6961, #16070, #18734, .T. ) ;
#7503 = CARTESIAN_POINT ( 'NONE',  ( 4.000698171653723101, 11.64110105645932691, 0.000000000000000000 ) ) ;
#7504 = CARTESIAN_POINT ( 'NONE',  ( 8.222191417683175629, -21.02099543870834353, 3.964901035250761208 ) ) ;
#7505 = CARTESIAN_POINT ( 'NONE',  ( -12.68288333306630378, -17.32689168014509207, 5.548858176248425700 ) ) ;
#7506 = CARTESIAN_POINT ( 'NONE',  ( -13.09030858231679417, -21.63647391050454871, 2.479004561291657804 ) ) ;
#7507 = CARTESIAN_POINT ( 'NONE',  ( -12.06594141768317741, -23.73192549717336064, 1.696391591240623331 ) ) ;
#7508 = ORIENTED_EDGE ( 'NONE', *, *, #4087, .T. ) ;
#7509 = CARTESIAN_POINT ( 'NONE',  ( 13.12529397354238192, 5.014845663890295846, 4.916666666666650087 ) ) ;
#7510 = CARTESIAN_POINT ( 'NONE',  ( -13.10372118337080849, 3.925419760224517329, 6.005889426248455010 ) ) ;
#7511 = ORIENTED_EDGE ( 'NONE', *, *, #8347, .F. ) ;
#7512 = DIRECTION ( 'NONE',  ( 1.000000000000000000, 0.000000000000000000, -0.000000000000000000 ) ) ;
#7513 = ORIENTED_EDGE ( 'NONE', *, *, #11530, .F. ) ;
#7514 = CARTESIAN_POINT ( 'NONE',  ( 0.5631383031621635116, -9.864917468222230923, 2.372643865078341019 ) ) ;
#7515 = EDGE_CURVE ( 'NONE', #19129, #5007, #16738, .T. ) ;
#7516 = ORIENTED_EDGE ( 'NONE', *, *, #16143, .T. ) ;
#7517 = LINE ( 'NONE', #12419, #13310 ) ;
#7518 = CARTESIAN_POINT ( 'NONE',  ( 26.04469207716615031, 9.000000000000001776, 0.000000000000000000 ) ) ;
#7519 = CARTESIAN_POINT ( 'NONE',  ( -2.031432063436913182, -10.08997855658269671, 1.680444048616273722 ) ) ;
#7520 = CARTESIAN_POINT ( 'NONE',  ( 2.499999999999999112, -24.49999999999999289, 4.000000000000000000 ) ) ;
#7521 = CARTESIAN_POINT ( 'NONE',  ( 15.00000000000001599, -18.49999999999999645, 4.000000000000000000 ) ) ;
#7522 = FACE_OUTER_BOUND ( 'NONE', #12224, .T. ) ;
#7523 = CARTESIAN_POINT ( 'NONE',  ( 12.44094141768317741, -20.19639159124061933, 1.768074502826635586 ) ) ;
#7524 = CARTESIAN_POINT ( 'NONE',  ( -13.12529418130016445, 5.014856155665242454, 4.958178834604180629 ) ) ;
#7525 = CARTESIAN_POINT ( 'NONE',  ( -10.09719141768317741, -22.77556120703057729, 5.229004561291655584 ) ) ;
#7526 = VERTEX_POINT ( 'NONE', #16841 ) ;
#7527 = CARTESIAN_POINT ( 'NONE',  ( 4.000698171653723101, 11.64110105645932691, 10.00000000000000000 ) ) ;
#7528 = DIRECTION ( 'NONE',  ( 0.000000000000000000, -1.000000000000000000, 0.000000000000000000 ) ) ;
#7529 = CARTESIAN_POINT ( 'NONE',  ( -13.37499964066394043, -21.00001814646822496, 4.442866346476199269 ) ) ;
#7530 = CARTESIAN_POINT ( 'NONE',  ( 9.809058582316794173, -23.27327832286945153, 2.298404588716537411 ) ) ;
#7531 = CARTESIAN_POINT ( 'NONE',  ( 27.94203811574921659, 9.999999999999998224, 0.000000000000000000 ) ) ;
#7532 = ORIENTED_EDGE ( 'NONE', *, *, #16136, .T. ) ;
#7533 = ORIENTED_EDGE ( 'NONE', *, *, #14609, .T. ) ;
#7534 = CARTESIAN_POINT ( 'NONE',  ( 13.41834698511420676, -18.81097725173551893, 6.252442769197418926 ) ) ;
#7535 = AXIS2_PLACEMENT_3D ( 'NONE', #1000, #7391, #19947 ) ;
#7536 = CARTESIAN_POINT ( 'NONE',  ( -9.305650798910056309, 0.000000000000000000, 1.000000000000000000 ) ) ;
#7537 = VECTOR ( 'NONE', #9234, 1000.000000000000000 ) ;
#7538 = FILL_AREA_STYLE_COLOUR ( '', #19400 ) ;
#7539 = ORIENTED_EDGE ( 'NONE', *, *, #11297, .T. ) ;
#7540 = EDGE_CURVE ( 'NONE', #3927, #20096, #16156, .T. ) ;
#7541 = CARTESIAN_POINT ( 'NONE',  ( -3.999999999999999112, -7.500000000000047073, 9.999999999999998224 ) ) ;
#7542 = ORIENTED_EDGE ( 'NONE', *, *, #8352, .T. ) ;
#7543 = CARTESIAN_POINT ( 'NONE',  ( 13.87470602645761986, 4.985154336109792972, 4.166666666666758445 ) ) ;
#7544 = CARTESIAN_POINT ( 'NONE',  ( 0.000000000000000000, 9.000000000000001776, 1.000000000000000000 ) ) ;
#7545 = CARTESIAN_POINT ( 'NONE',  ( 2.780192134145684779, -10.08406280675441735, 1.871539748636713130 ) ) ;
#7546 = LINE ( 'NONE', #13598, #10391 ) ;
#7547 = CARTESIAN_POINT ( 'NONE',  ( -13.09560264576187905, 4.265433610975056133, 4.583333333333295734 ) ) ;
#7548 = AXIS2_PLACEMENT_3D ( 'NONE', #6238, #11058, #15953 ) ;
#7549 = DIRECTION ( 'NONE',  ( 1.000000000000000000, 0.000000000000000000, -0.000000000000000000 ) ) ;
#7550 = CARTESIAN_POINT ( 'NONE',  ( -13.86676110481170632, 3.833935792988865110, 6.739421935864088553 ) ) ;
#7551 = CARTESIAN_POINT ( 'NONE',  ( 19.73630159782011617, 0.000000000000000000, 1.000000000000000000 ) ) ;
#7552 = CARTESIAN_POINT ( 'NONE',  ( 11.02780858231679595, -23.72900456129165647, 4.275561207030568411 ) ) ;
#7553 = CARTESIAN_POINT ( 'NONE',  ( 11.78469141768317741, -23.02099543870834353, 3.863526089495429972 ) ) ;
#7554 = CARTESIAN_POINT ( 'NONE',  ( -12.15969141768317563, -22.67418626127524917, 1.729004561291651587 ) ) ;
#7555 = EDGE_LOOP ( 'NONE', ( #1774, #19987, #1531, #14561 ) ) ;
#7556 = CARTESIAN_POINT ( 'NONE',  ( 13.74418849449709512, -0.8559810278826442964, 5.138499963383082125 ) ) ;
#7557 = FACE_OUTER_BOUND ( 'NONE', #4275, .T. ) ;
#7558 = ORIENTED_EDGE ( 'NONE', *, *, #7997, .F. ) ;
#7559 = EDGE_LOOP ( 'NONE', ( #18202, #14334, #8081, #19198, #15646, #10311 ) ) ;
#7560 = CARTESIAN_POINT ( 'NONE',  ( -5.381197846483055436, -6.000000000000000000, 2.000000000000000000 ) ) ;
#7561 = EDGE_CURVE ( 'NONE', #11536, #7887, #18815, .T. ) ;
#7562 = CARTESIAN_POINT ( 'NONE',  ( -13.08573665985359824, 3.017201322601628100, 5.986358176248492313 ) ) ;
#7563 = CARTESIAN_POINT ( 'NONE',  ( -2.367358971471363649, -9.400572650371021410, 2.446005822389718087 ) ) ;
#7564 = CARTESIAN_POINT ( 'NONE',  ( -13.40621837757088564, -18.67347193267085714, 5.505367199623145247 ) ) ;
#7565 = EDGE_CURVE ( 'NONE', #11462, #7606, #13692, .T. ) ;
#7566 = CARTESIAN_POINT ( 'NONE',  ( 17.80017143803810242, 4.999999999999999112, 1.000000000000000000 ) ) ;
#7567 = FACE_OUTER_BOUND ( 'NONE', #8998, .T. ) ;
#7568 = DIRECTION ( 'NONE',  ( 1.000000000000000000, 0.000000000000000000, 0.000000000000000000 ) ) ;
#7569 = ADVANCED_FACE ( 'NONE', ( #4088 ), #15266, .F. ) ;
#7570 = CARTESIAN_POINT ( 'NONE',  ( 11.00000000000000000, -24.49999999999999289, 5.000000000000000000 ) ) ;
#7571 = DIRECTION ( 'NONE',  ( -0.000000000000000000, -0.000000000000000000, -1.000000000000000000 ) ) ;
#7572 = CARTESIAN_POINT ( 'NONE',  ( -9.715308582316795949, -24.52099543870834708, 2.515153566944913432 ) ) ;
#7573 = CARTESIAN_POINT ( 'NONE',  ( -2.739050625766161762, -9.875938058683834342, 1.818089155622620412 ) ) ;
#7574 = ORIENTED_EDGE ( 'NONE', *, *, #6039, .F. ) ;
#7575 = CARTESIAN_POINT ( 'NONE',  ( -13.37499979530394967, -20.25001033714808329, 4.458488164327452097 ) ) ;
#7576 = DIRECTION ( 'NONE',  ( -0.000000000000000000, -0.000000000000000000, -1.000000000000000000 ) ) ;
#7577 = CARTESIAN_POINT ( 'NONE',  ( 6.621558582316796837, -24.50000000000000000, 3.550687472877651629 ) ) ;
#7578 = CARTESIAN_POINT ( 'NONE',  ( -4.190941417683176518, -22.74294823697955081, 4.171265325393542334 ) ) ;
#7579 = ORIENTED_EDGE ( 'NONE', *, *, #11635, .F. ) ;
#7580 = CARTESIAN_POINT ( 'NONE',  ( 13.87406079471522347, 4.952570133121557028, 5.260711232101737522 ) ) ;
#7581 = LINE ( 'NONE', #17196, #11063 ) ;
#7582 = ORIENTED_EDGE ( 'NONE', *, *, #17515, .T. ) ;
#7583 = ORIENTED_EDGE ( 'NONE', *, *, #16202, .F. ) ;
#7584 = CARTESIAN_POINT ( 'NONE',  ( 13.00209451496117374, 10.00000000000000000, 0.000000000000000000 ) ) ;
#7585 = ORIENTED_EDGE ( 'NONE', *, *, #12949, .F. ) ;
#7586 = CARTESIAN_POINT ( 'NONE',  ( -13.87470586348985258, 4.985146106231644225, 5.033049509202228933 ) ) ;
#7587 = ADVANCED_FACE ( 'NONE', ( #18527 ), #7637, .T. ) ;
#7588 = CARTESIAN_POINT ( 'NONE',  ( -22.81633994409548549, 16.00000000000000000, 1.000000000000000000 ) ) ;
#7589 = ORIENTED_EDGE ( 'NONE', *, *, #9972, .F. ) ;
#7590 = FACE_OUTER_BOUND ( 'NONE', #14666, .T. ) ;
#7591 = DIRECTION ( 'NONE',  ( -1.000000000000000000, -0.000000000000000000, -0.000000000000000000 ) ) ;
#7592 = LINE ( 'NONE', #20158, #8331 ) ;
#7593 = CARTESIAN_POINT ( 'NONE',  ( 2.506848361495492394, -9.459347215042898327, 1.711100304737409150 ) ) ;
#7594 = CARTESIAN_POINT ( 'NONE',  ( 15.06494360078803041, 11.64110105645932691, 0.000000000000000000 ) ) ;
#7595 = CARTESIAN_POINT ( 'NONE',  ( 0.000000000000000000, 9.000000000000001776, 0.000000000000000000 ) ) ;
#7596 = FACE_OUTER_BOUND ( 'NONE', #19175, .T. ) ;
#7597 = DIRECTION ( 'NONE',  ( 1.000000000000000000, -3.469446951953491127E-15, 0.000000000000000000 ) ) ;
#7598 = PLANE ( 'NONE',  #3696 ) ;
#7599 = CARTESIAN_POINT ( 'NONE',  ( 3.974842109207560537, -21.92432777746334693, 4.506404853634142782 ) ) ;
#7600 = CARTESIAN_POINT ( 'NONE',  ( -13.12526104302547836, 5.013182672784613381, 5.066812735559260261 ) ) ;
#7601 = EDGE_CURVE ( 'NONE', #18502, #1851, #13590, .T. ) ;
#7602 = CARTESIAN_POINT ( 'NONE',  ( -9.809058582316795949, -22.74294823697954016, 2.828734674606448785 ) ) ;
#7603 = CARTESIAN_POINT ( 'NONE',  ( -8.784691417683177406, -24.52099543870834708, 4.484846433055073689 ) ) ;
#7604 = ORIENTED_EDGE ( 'NONE', *, *, #4237, .T. ) ;
#7605 = CARTESIAN_POINT ( 'NONE',  ( 13.01365964058540037, 0.1273118495903458325, 5.174178440007729307 ) ) ;
#7606 = VERTEX_POINT ( 'NONE', #19993 ) ;
#7607 = LINE ( 'NONE', #17123, #10970 ) ;
#7608 = VERTEX_POINT ( 'NONE', #9206 ) ;
#7609 = CARTESIAN_POINT ( 'NONE',  ( 2.011668220304084542, -11.03559989230542193, 2.673298498313999794 ) ) ;
#7610 = EDGE_CURVE ( 'NONE', #2724, #11847, #12027, .T. ) ;
#7611 = EDGE_CURVE ( 'NONE', #16180, #20415, #16939, .T. ) ;
#7612 = ORIENTED_EDGE ( 'NONE', *, *, #20355, .T. ) ;
#7613 = FACE_OUTER_BOUND ( 'NONE', #101, .T. ) ;
#7614 = CARTESIAN_POINT ( 'NONE',  ( -1.561130159782011306, 9.000000000000001776, 1.000000000000000000 ) ) ;
#7615 = CARTESIAN_POINT ( 'NONE',  ( -1.991511895312070957, -10.01421418592441448, 1.660986244685804136 ) ) ;
#7616 = FACE_OUTER_BOUND ( 'NONE', #16226, .T. ) ;
#7617 = LINE ( 'NONE', #15767, #16972 ) ;
#7618 = CARTESIAN_POINT ( 'NONE',  ( 27.94203811574921303, 11.64110105645932691, 0.000000000000000000 ) ) ;
#7619 = CARTESIAN_POINT ( 'NONE',  ( 4.565941417683176518, -23.73192549717336064, 1.696391591240623331 ) ) ;
#7620 = CARTESIAN_POINT ( 'NONE',  ( -13.12529397354238192, 5.014845663890295846, 4.583333333333296622 ) ) ;
#7621 = VECTOR ( 'NONE', #13462, 1000.000000000000000 ) ;
#7622 = CARTESIAN_POINT ( 'NONE',  ( -11.50344141768317563, -22.05068747287765873, 5.250000000000000888 ) ) ;
#7623 =( BOUNDED_CURVE ( )  B_SPLINE_CURVE ( 3, ( #6835, #17719, #13204, #8300 ),
 .UNSPECIFIED., .F., .F. ) 
 B_SPLINE_CURVE_WITH_KNOTS ( ( 4, 4 ),
 ( 1.468430546537837468E-05, 0.001172421487176120289 ),
 .UNSPECIFIED. ) 
 CURVE ( )  GEOMETRIC_REPRESENTATION_ITEM ( )  RATIONAL_B_SPLINE_CURVE ( ( 0.9619191252709937690, 0.3335846922424353656, 0.3462783171521043313, 1.000000000000000222 ) ) 
 REPRESENTATION_ITEM ( '' )  );
#7624 = ORIENTED_EDGE ( 'NONE', *, *, #6218, .F. ) ;
#7625 = CARTESIAN_POINT ( 'NONE',  ( 9.340308582316794173, -22.67418626127525982, 5.270995438708342640 ) ) ;
#7626 = CARTESIAN_POINT ( 'NONE',  ( -20.00349085826861995, 11.64110105645932691, 10.00000000000000000 ) ) ;
#7627 = CARTESIAN_POINT ( 'NONE',  ( -13.90439735423812273, 5.734566389025032684, 4.166666666666765551 ) ) ;
#7628 = CARTESIAN_POINT ( 'NONE',  ( 8.309058582316792396, -23.27327832286945153, 2.298404588716537411 ) ) ;
#7629 = PLANE ( 'NONE',  #10668 ) ;
#7630 = EDGE_LOOP ( 'NONE', ( #10731, #10931, #11082, #385 ) ) ;
#7631 = VERTEX_POINT ( 'NONE', #14008 ) ;
#7632 = CARTESIAN_POINT ( 'NONE',  ( 13.37607268932110038, -20.94582918928111681, 4.945564004704174010 ) ) ;
#7633 = VECTOR ( 'NONE', #17022, 1000.000000000000000 ) ;
#7634 = CARTESIAN_POINT ( 'NONE',  ( -17.11324865405191176, -11.00000000000000000, 1.000000000000000000 ) ) ;
#7635 = ORIENTED_EDGE ( 'NONE', *, *, #15537, .T. ) ;
#7636 = VECTOR ( 'NONE', #19749, 1000.000000000000000 ) ;
#7637 = PLANE ( 'NONE',  #6121 ) ;
#7638 = VECTOR ( 'NONE', #9924, 1000.000000000000000 ) ;
#7639 = VERTEX_POINT ( 'NONE', #2508 ) ;
#7640 = CARTESIAN_POINT ( 'NONE',  ( -9.527808582316792396, -23.72900456129165647, 4.275561207030568411 ) ) ;
#7641 = CARTESIAN_POINT ( 'NONE',  ( -17.05017143803810242, 9.000000000000001776, 1.000000000000000000 ) ) ;
#7642 = DIRECTION ( 'NONE',  ( -1.000000000000000000, 0.000000000000000000, 0.000000000000000000 ) ) ;
#7643 = CARTESIAN_POINT ( 'NONE',  ( 3.486710468562268961, -9.848741751643258269, 2.003719583429115492 ) ) ;
#7644 = DIRECTION ( 'NONE',  ( 0.000000000000000000, -1.000000000000000000, 0.000000000000000000 ) ) ;
#7645 = CARTESIAN_POINT ( 'NONE',  ( -13.37499999998404299, -19.49999999996810729, 2.793053905886972998 ) ) ;
#7646 = AXIS2_PLACEMENT_3D ( 'NONE', #3702, #11446, #5069 ) ;
#7647 = CARTESIAN_POINT ( 'NONE',  ( 6.809058582316794173, -23.27327832286945153, 2.298404588716537411 ) ) ;
#7648 = CARTESIAN_POINT ( 'NONE',  ( -13.88045627189955233, 4.525541730927888473, 6.662882075361062029 ) ) ;
#7649 = EDGE_CURVE ( 'NONE', #19969, #18281, #12339, .T. ) ;
#7650 = VECTOR ( 'NONE', #9675, 1000.000000000000000 ) ;
#7651 = LINE ( 'NONE', #9320, #7730 ) ;
#7652 = CARTESIAN_POINT ( 'NONE',  ( 12.71530858231679240, -23.77099543870833998, 2.825813738724734847 ) ) ;
#7653 = AXIS2_PLACEMENT_3D ( 'NONE', #20077, #20389, #16917 ) ;
#7654 = CARTESIAN_POINT ( 'NONE',  ( 9.628441417683177406, -20.99999999999999645, 3.550687472877664952 ) ) ;
#7655 = CARTESIAN_POINT ( 'NONE',  ( -10.00344141768317563, -22.05068747287765873, 5.250000000000000888 ) ) ;
#7656 = ORIENTED_EDGE ( 'NONE', *, *, #3038, .T. ) ;
#7657 = CARTESIAN_POINT ( 'NONE',  ( 13.37499999999998224, -19.49999999999991473, 4.333333333333343695 ) ) ;
#7658 = CARTESIAN_POINT ( 'NONE',  ( -2.682825141213236009, -9.727160171598653093, 1.779880022082258373 ) ) ;
#7659 = ORIENTED_EDGE ( 'NONE', *, *, #3263, .T. ) ;
#7660 = VERTEX_POINT ( 'NONE', #13801 ) ;
#7661 = DIRECTION ( 'NONE',  ( 1.000000000000000000, 0.000000000000000000, 0.000000000000000000 ) ) ;
#7662 = AXIS2_PLACEMENT_3D ( 'NONE', #6441, #12806, #13011 ) ;
#7663 = VECTOR ( 'NONE', #17856, 1000.000000000000000 ) ;
#7664 = CARTESIAN_POINT ( 'NONE',  ( -20.00000000000000000, -0.5000000000000004441, 0.5000000000000000000 ) ) ;
#7665 = AXIS2_PLACEMENT_3D ( 'NONE', #5111, #98, #9917 ) ;
#7666 = CARTESIAN_POINT ( 'NONE',  ( -1.337453470010121714, -8.364917468222230923, 2.372643865078341019 ) ) ;
#7667 = CARTESIAN_POINT ( 'NONE',  ( -13.40022353639839103, -18.97621141187856608, 5.498856782956575984 ) ) ;
#7668 = CARTESIAN_POINT ( 'NONE',  ( 23.10856191738414012, 4.999999999999999112, 0.000000000000000000 ) ) ;
#7669 = CARTESIAN_POINT ( 'NONE',  ( 14.50000000000000000, -23.00000000000001421, 4.000000000000000000 ) ) ;
#7670 = CARTESIAN_POINT ( 'NONE',  ( 11.00000000000000000, -23.83493649053891517, 4.999999999999999112 ) ) ;
#7671 = LINE ( 'NONE', #20029, #6406 ) ;
#7672 = CARTESIAN_POINT ( 'NONE',  ( -11.96530858231679773, -19.47900456129164937, 4.484846433055089676 ) ) ;
#7673 = CARTESIAN_POINT ( 'NONE',  ( -0.9854920305337622199, -8.364917468222230923, 1.622643865078341907 ) ) ;
#7674 = ORIENTED_EDGE ( 'NONE', *, *, #7398, .T. ) ;
#7675 = VECTOR ( 'NONE', #13643, 1000.000000000000000 ) ;
#7676 = CARTESIAN_POINT ( 'NONE',  ( -13.84501469867711698, 4.235742283194553259, 4.583333333333295734 ) ) ;
#7677 = DIRECTION ( 'NONE',  ( 0.000000000000000000, 0.000000000000000000, 1.000000000000000000 ) ) ;
#7678 = EDGE_CURVE ( 'NONE', #14333, #11513, #12456, .T. ) ;
#7679 = CARTESIAN_POINT ( 'NONE',  ( 4.687312169500634340, -21.32903648725300272, 5.908812401261035241 ) ) ;
#7680 = CARTESIAN_POINT ( 'NONE',  ( -12.43405858231679595, -22.67126532539354855, 4.242948236979545484 ) ) ;
#7681 = AXIS2_PLACEMENT_3D ( 'NONE', #7958, #14332, #9326 ) ;
#7682 = EDGE_LOOP ( 'NONE', ( #11972, #16575, #3087, #10720 ) ) ;
#7683 = CARTESIAN_POINT ( 'NONE',  ( 13.40995420747273670, -19.23481252262645924, 6.243328185864100988 ) ) ;
#7684 = DIRECTION ( 'NONE',  ( 0.000000000000000000, -0.000000000000000000, 1.000000000000000000 ) ) ;
#7685 = ORIENTED_EDGE ( 'NONE', *, *, #9276, .F. ) ;
#7686 = ORIENTED_EDGE ( 'NONE', *, *, #9232, .T. ) ;
#7687 = FACE_OUTER_BOUND ( 'NONE', #12180, .T. ) ;
#7688 = AXIS2_PLACEMENT_3D ( 'NONE', #10992, #2, #3242 ) ;
#7689 = ORIENTED_EDGE ( 'NONE', *, *, #3638, .F. ) ;
#7690 = CARTESIAN_POINT ( 'NONE',  ( -13.85593616229004610, 4.037276195647738319, 5.992122970672676630 ) ) ;
#7691 = EDGE_CURVE ( 'NONE', #20689, #12892, #20303, .T. ) ;
#7692 = DIRECTION ( 'NONE',  ( 0.000000000000000000, 1.000000000000000000, -0.000000000000000000 ) ) ;
#7693 = EDGE_LOOP ( 'NONE', ( #9298, #7821, #8823, #20097 ) ) ;
#7694 = CARTESIAN_POINT ( 'NONE',  ( 19.23630159782011617, 0.000000000000000000, 0.000000000000000000 ) ) ;
#7695 = CARTESIAN_POINT ( 'NONE',  ( 7.619520639128047002, 9.000000000000001776, 1.000000000000000000 ) ) ;
#7696 = STYLED_ITEM ( 'NONE', ( #15168 ), #10808 ) ;
#7697 = CARTESIAN_POINT ( 'NONE',  ( -0.000000000000000000, 11.64110105645932691, 0.000000000000000000 ) ) ;
#7698 = CARTESIAN_POINT ( 'NONE',  ( 1.126276606324276619, -8.364917468222230923, 1.622643865078341907 ) ) ;
#7699 = CARTESIAN_POINT ( 'NONE',  ( 24.50000000000000000, 0.000000000000000000, 1.000000000000000000 ) ) ;
#7700 = FACE_OUTER_BOUND ( 'NONE', #14085, .T. ) ;
#7701 = VECTOR ( 'NONE', #16624, 1000.000000000000000 ) ;
#7702 = DIRECTION ( 'NONE',  ( -1.000000000000000000, -0.000000000000000000, -0.000000000000000000 ) ) ;
#7703 = DIRECTION ( 'NONE',  ( 0.000000000000000000, 0.000000000000000000, -1.000000000000000000 ) ) ;
#7704 = CARTESIAN_POINT ( 'NONE',  ( 13.12529397354238192, 5.014845663890295846, 4.583333333333296622 ) ) ;
#7705 = CARTESIAN_POINT ( 'NONE',  ( 5.034691417683177406, -20.97900456129164581, 3.136473910504570917 ) ) ;
#7706 = CARTESIAN_POINT ( 'NONE',  ( -13.09293046926041626, 3.380488697651010011, 5.994170676248444352 ) ) ;
#7707 = CARTESIAN_POINT ( 'NONE',  ( -9.059058582316795949, -21.25705176302045274, 4.171265325393551215 ) ) ;
#7708 = EDGE_CURVE ( 'NONE', #7379, #5682, #14419, .T. ) ;
#7709 = CARTESIAN_POINT ( 'NONE',  ( -5.878441417683177406, -24.50000000000000000, 3.449312527122335048 ) ) ;
#7710 = ORIENTED_EDGE ( 'NONE', *, *, #18846, .T. ) ;
#7711 = CARTESIAN_POINT ( 'NONE',  ( 13.37499999999998224, -19.49999999999998934, 4.291666666666699825 ) ) ;
#7712 = CARTESIAN_POINT ( 'NONE',  ( 5.000000000000000000, -12.50000000000000000, 4.500000000000000888 ) ) ;
#7713 = EDGE_LOOP ( 'NONE', ( #9390, #403, #12156, #10098 ) ) ;
#7714 = CARTESIAN_POINT ( 'NONE',  ( -7.499999999999999112, -24.49999999999999289, 4.000000000000000000 ) ) ;
#7715 = ORIENTED_EDGE ( 'NONE', *, *, #9847, .F. ) ;
#7716 = CARTESIAN_POINT ( 'NONE',  ( 1.337453470010121714, -9.864917468222230923, 2.372643865078341019 ) ) ;
#7717 = EDGE_CURVE ( 'NONE', #2830, #2924, #11186, .T. ) ;
#7718 = AXIS2_PLACEMENT_3D ( 'NONE', #7551, #8814, #2629 ) ;
#7719 = EDGE_CURVE ( 'NONE', #19250, #4026, #1562, .T. ) ;
#7720 = VECTOR ( 'NONE', #16178, 1000.000000000000000 ) ;
#7721 = VECTOR ( 'NONE', #1912, 1000.000000000000000 ) ;
#7722 = VECTOR ( 'NONE', #20212, 1000.000000000000000 ) ;
#7723 = VERTEX_POINT ( 'NONE', #1367 ) ;
#7724 = CARTESIAN_POINT ( 'NONE',  ( 25.37918902992234393, 0.000000000000000000, 0.000000000000000000 ) ) ;
#7725 = CARTESIAN_POINT ( 'NONE',  ( 2.311130159782011972, 0.000000000000000000, 1.000000000000000000 ) ) ;
#7726 = CARTESIAN_POINT ( 'NONE',  ( -2.057814715640970515, -10.20705538578787852, 1.710511717200805304 ) ) ;
#7727 = CARTESIAN_POINT ( 'NONE',  ( 15.86404127825609400, 0.000000000000000000, 1.000000000000000000 ) ) ;
#7728 = LINE ( 'NONE', #3019, #11306 ) ;
#7729 = LINE ( 'NONE', #6158, #5575 ) ;
#7730 = VECTOR ( 'NONE', #12551, 1000.000000000000000 ) ;
#7731 = CARTESIAN_POINT ( 'NONE',  ( 7.097191417683176518, -23.08622137881040359, 5.979004561291654696 ) ) ;
#7732 = SURFACE_SIDE_STYLE ('',( #2915 ) ) ;
#7733 = CARTESIAN_POINT ( 'NONE',  ( -7.659691417683177406, -22.67418626127524917, 1.729004561291651809 ) ) ;
#7734 = VECTOR ( 'NONE', #10266, 1000.000000000000000 ) ;
#7735 = EDGE_CURVE ( 'NONE', #6964, #13772, #1465, .T. ) ;
#7736 = VERTEX_POINT ( 'NONE', #19251 ) ;
#7737 = CARTESIAN_POINT ( 'NONE',  ( 9.996558582316794173, -22.05068747287764452, 1.749999999999998446 ) ) ;
#7738 = CARTESIAN_POINT ( 'NONE',  ( 9.555650798910054533, 9.000000000000001776, 1.000000000000000000 ) ) ;
#7739 = CARTESIAN_POINT ( 'NONE',  ( -13.90439771357353038, 5.734584535470497180, 4.942866369314573127 ) ) ;
#7740 = VERTEX_POINT ( 'NONE', #4501 ) ;
#7741 = VECTOR ( 'NONE', #18144, 1000.000000000000000 ) ;
#7742 = CARTESIAN_POINT ( 'NONE',  ( 6.809058582316794173, -23.27327832286945153, 2.298404588716537411 ) ) ;
#7743 = DIRECTION ( 'NONE',  ( 1.000000000000000000, 0.000000000000000000, -0.000000000000000000 ) ) ;
#7744 = ORIENTED_EDGE ( 'NONE', *, *, #10013, .F. ) ;
#7745 = LINE ( 'NONE', #18935, #7266 ) ;
#7746 = ORIENTED_EDGE ( 'NONE', *, *, #16689, .F. ) ;
#7747 = CARTESIAN_POINT ( 'NONE',  ( -8.376396343307449754, 0.000000000000000000, 0.000000000000000000 ) ) ;
#7748 = ORIENTED_EDGE ( 'NONE', *, *, #6694, .T. ) ;
#7749 = EDGE_CURVE ( 'NONE', #9890, #5036, #9607, .T. ) ;
#7750 = CARTESIAN_POINT ( 'NONE',  ( -12.34030858231679240, -22.67418626127525982, 5.270995438708342640 ) ) ;
#7751 = CARTESIAN_POINT ( 'NONE',  ( 12.63819864697926754, -19.58346832754827105, 5.450273968536036406 ) ) ;
#7752 = DIRECTION ( 'NONE',  ( 1.000000000000000000, 0.000000000000000000, 0.000000000000000000 ) ) ;
#7753 = CARTESIAN_POINT ( 'NONE',  ( 1.548630333695928618, -8.364917468222230923, 1.622643865078341907 ) ) ;
#7754 = LINE ( 'NONE', #20425, #2330 ) ;
#7755 = CARTESIAN_POINT ( 'NONE',  ( -13.09560264576187905, 4.265433610975056133, 4.916666666666649199 ) ) ;
#7756 = CARTESIAN_POINT ( 'NONE',  ( 5.965308582316793284, -20.22900456129164937, 4.174186261275266929 ) ) ;
#7757 = CARTESIAN_POINT ( 'NONE',  ( -13.90439735423812273, 5.734566389025032684, 4.583333333333295734 ) ) ;
#7758 = EDGE_CURVE ( 'NONE', #4108, #19480, #9511, .T. ) ;
#7759 = EDGE_CURVE ( 'NONE', #18720, #4492, #14307, .T. ) ;
#7760 = CARTESIAN_POINT ( 'NONE',  ( -13.15332036705482466, 5.722234611034569873, 3.999999999999985345 ) ) ;
#7761 = CARTESIAN_POINT ( 'NONE',  ( 7.840308582316794173, -22.67418626127525982, 5.270995438708342640 ) ) ;
#7762 = VECTOR ( 'NONE', #11037, 1000.000000000000000 ) ;
#7763 = CARTESIAN_POINT ( 'NONE',  ( 12.71530858231679417, -23.02099543870833998, 3.136473910504556262 ) ) ;
#7764 = CARTESIAN_POINT ( 'NONE',  ( -6.902808582316793284, -22.77556120703056308, 1.770995438708339975 ) ) ;
#7765 = ORIENTED_EDGE ( 'NONE', *, *, #17591, .F. ) ;
#7766 = CARTESIAN_POINT ( 'NONE',  ( 13.38007464613909470, -19.24373036997283037, 4.743072998953621777 ) ) ;
#7767 = CARTESIAN_POINT ( 'NONE',  ( -16.62779268661489951, 16.00000000000000000, 1.000000000000000000 ) ) ;
#7768 = ORIENTED_EDGE ( 'NONE', *, *, #14481, .T. ) ;
#7769 = UNCERTAINTY_MEASURE_WITH_UNIT (LENGTH_MEASURE( 1.000000000000000082E-05 ), #18732, 'distance_accuracy_value', 'NONE');
#7770 = VECTOR ( 'NONE', #230, 1000.000000000000000 ) ;
#7771 = ORIENTED_EDGE ( 'NONE', *, *, #10492, .F. ) ;
#7772 = DIRECTION ( 'NONE',  ( -0.000000000000000000, 0.000000000000000000, -1.000000000000000000 ) ) ;
#7773 = EDGE_CURVE ( 'NONE', #4874, #17458, #11090, .T. ) ;
#7774 = CARTESIAN_POINT ( 'NONE',  ( -12.62503117662529739, -20.24842558042254836, 4.565011198945062354 ) ) ;
#7775 = CARTESIAN_POINT ( 'NONE',  ( -1.619022621591187150, -9.114917468222230923, 2.372643865078341019 ) ) ;
#7776 = CARTESIAN_POINT ( 'NONE',  ( -13.44218742460511073, -16.85703505742523234, 5.544429699623282914 ) ) ;
#7777 = AXIS2_PLACEMENT_3D ( 'NONE', #6513, #1698, #7866 ) ;
#7778 = LINE ( 'NONE', #20642, #4709 ) ;
#7779 = LINE ( 'NONE', #13930, #10884 ) ;
#7780 = DIRECTION ( 'NONE',  ( 1.000000000000000000, 0.000000000000000000, 0.000000000000000000 ) ) ;
#7781 = CARTESIAN_POINT ( 'NONE',  ( -15.49999999999999822, -22.99999999999999289, 1.000000000000000000 ) ) ;
#7782 = CARTESIAN_POINT ( 'NONE',  ( 13.13084019862132479, 4.544930030374419339, 6.677052771569639944 ) ) ;
#7783 = CARTESIAN_POINT ( 'NONE',  ( -10.84719141768317741, -20.91377862118959285, 1.020995438708345082 ) ) ;
#7784 = CARTESIAN_POINT ( 'NONE',  ( -2.155282726790247239, -12.05525952636828357, 2.935167462089139256 ) ) ;
#7785 = ORIENTED_EDGE ( 'NONE', *, *, #9483, .T. ) ;
#7786 = CARTESIAN_POINT ( 'NONE',  ( -13.39359219590679295, -19.31109410670777038, 5.491647114909025795 ) ) ;
#7787 = DIRECTION ( 'NONE',  ( 1.000000000000000000, 0.000000000000000000, -0.000000000000000000 ) ) ;
#7788 = CARTESIAN_POINT ( 'NONE',  ( 8.034691417683175629, -19.47900456129164581, 2.515153566944927199 ) ) ;
#7789 = CARTESIAN_POINT ( 'NONE',  ( -12.24655858231679595, -21.94931252712234127, 4.499999999999999112 ) ) ;
#7790 = ORIENTED_EDGE ( 'NONE', *, *, #8472, .F. ) ;
#7791 = CARTESIAN_POINT ( 'NONE',  ( 13.39169349927020569, -20.15697828685464188, 6.009339318877812808 ) ) ;
#7792 = CARTESIAN_POINT ( 'NONE',  ( 12.63465172146706728, -19.76258806590802664, 5.372658420469845986 ) ) ;
#7793 = DIRECTION ( 'NONE',  ( -0.000000000000000000, 0.000000000000000000, -1.000000000000000000 ) ) ;
#7794 = ORIENTED_EDGE ( 'NONE', *, *, #18860, .T. ) ;
#7795 = VECTOR ( 'NONE', #20102, 1000.000000000000000 ) ;
#7796 = ORIENTED_EDGE ( 'NONE', *, *, #18103, .T. ) ;
#7797 = CARTESIAN_POINT ( 'NONE',  ( -13.87215786865436762, 4.856472367046606564, 5.506273593909547515 ) ) ;
#7798 = EDGE_CURVE ( 'NONE', #8356, #15336, #9308, .T. ) ;
#7799 = CARTESIAN_POINT ( 'NONE',  ( 1.957016269584227031, -9.152392576945766578, 2.382268221639079364 ) ) ;
#7800 = PLANE ( 'NONE',  #8972 ) ;
#7801 = CARTESIAN_POINT ( 'NONE',  ( -9.689245429134309973, 16.00000000000000000, 1.000000000000000000 ) ) ;
#7802 = FACE_OUTER_BOUND ( 'NONE', #12179, .T. ) ;
#7803 = FACE_OUTER_BOUND ( 'NONE', #16483, .T. ) ;
#7804 = CARTESIAN_POINT ( 'NONE',  ( 1.548630333695928396, -9.114917468222230923, 1.622643865078341463 ) ) ;
#7805 = CARTESIAN_POINT ( 'NONE',  ( -24.12918902992234393, 11.64110105645932691, 0.000000000000000000 ) ) ;
#7806 = CARTESIAN_POINT ( 'NONE',  ( 10.93924542913430820, 10.00000000000000000, 1.000000000000000000 ) ) ;
#7807 = CYLINDRICAL_SURFACE ( 'NONE', #13293, 10.00000000000000000 ) ;
#7808 = FACE_OUTER_BOUND ( 'NONE', #12207, .T. ) ;
#7809 = CARTESIAN_POINT ( 'NONE',  ( -11.99999999999999467, -17.50000000000000000, 4.000000000000000000 ) ) ;
#7810 = CARTESIAN_POINT ( 'NONE',  ( 8.784691417683177406, -23.02099543870834353, 3.863526089495429972 ) ) ;
#7811 = CARTESIAN_POINT ( 'NONE',  ( -12.72125031657057015, -15.38935901321805133, 5.590524842915047365 ) ) ;
#7812 = CARTESIAN_POINT ( 'NONE',  ( -12.34030858231679773, -22.36352608949544418, 4.520995438708343528 ) ) ;
#7813 = CARTESIAN_POINT ( 'NONE',  ( -4.940941417683177406, -20.19639159124061933, 1.768074502826635586 ) ) ;
#7814 = ORIENTED_EDGE ( 'NONE', *, *, #11983, .T. ) ;
#7815 = CARTESIAN_POINT ( 'NONE',  ( 13.09560264576187905, 4.265433610975056133, 3.666666666666500873 ) ) ;
#7816 = CARTESIAN_POINT ( 'NONE',  ( -7.499999999999999112, -19.49999999999999645, 4.000000000000000000 ) ) ;
#7817 = ORIENTED_EDGE ( 'NONE', *, *, #9887, .F. ) ;
#7818 = CARTESIAN_POINT ( 'NONE',  ( -27.00000000000000000, 0.000000000000000000, 1.000000000000000000 ) ) ;
#7819 = ORIENTED_EDGE ( 'NONE', *, *, #5577, .T. ) ;
#7820 = CARTESIAN_POINT ( 'NONE',  ( 1.548630333695928618, -9.864917468222230923, 2.372643865078341019 ) ) ;
#7821 = ORIENTED_EDGE ( 'NONE', *, *, #18109, .T. ) ;
#7822 = CARTESIAN_POINT ( 'NONE',  ( 12.06594141768317563, -23.20159541128344927, 2.226721677130534705 ) ) ;
#7823 = FACE_OUTER_BOUND ( 'NONE', #19961, .T. ) ;
#7824 = EDGE_CURVE ( 'NONE', #2297, #10229, #103, .T. ) ;
#7825 = CARTESIAN_POINT ( 'NONE',  ( -1.863950040896528604, -9.995453039732266731, 2.406168007552154098 ) ) ;
#7826 = CARTESIAN_POINT ( 'NONE',  ( 11.00000000000000000, -24.49999999999999289, 4.000000000000000000 ) ) ;
#7827 = CARTESIAN_POINT ( 'NONE',  ( -8.684058582316794173, -20.79840458871652942, 2.226721677130544030 ) ) ;
#7828 = EDGE_CURVE ( 'NONE', #16888, #7956, #16103, .T. ) ;
#7829 = EDGE_CURVE ( 'NONE', #8633, #10619, #15683, .T. ) ;
#7830 = CARTESIAN_POINT ( 'NONE',  ( 8.222191417683175629, -19.52099543870834353, 4.586221378810406257 ) ) ;
#7831 = CARTESIAN_POINT ( 'NONE',  ( 7.500000000000002665, -9.999999999999991118, 2.000000000000000000 ) ) ;
#7832 = CARTESIAN_POINT ( 'NONE',  ( -8.128441417683175629, -20.24999999999999289, 3.550687472877664952 ) ) ;
#7833 = ORIENTED_EDGE ( 'NONE', *, *, #1962, .T. ) ;
#7834 = CARTESIAN_POINT ( 'NONE',  ( 9.715308582316794173, -23.77099543870833998, 2.825813738724734847 ) ) ;
#7835 = CARTESIAN_POINT ( 'NONE',  ( 11.99178095869207006, 9.000000000000001776, 1.000000000000000000 ) ) ;
#7836 = CARTESIAN_POINT ( 'NONE',  ( -12.62499999999998224, -20.99999999999991829, 4.333333333333343695 ) ) ;
#7837 = VERTEX_POINT ( 'NONE', #20519 ) ;
#7838 = CARTESIAN_POINT ( 'NONE',  ( 9.246558582316794173, -21.94931252712234482, 5.250000000000000888 ) ) ;
#7839 = FACE_OUTER_BOUND ( 'NONE', #8106, .T. ) ;
#7840 = ORIENTED_EDGE ( 'NONE', *, *, #19877, .F. ) ;
#7841 = PRODUCT_DEFINITION_SHAPE ( 'NONE', 'NONE',  #9828 ) ;
#7842 = CARTESIAN_POINT ( 'NONE',  ( -2.693754455098655409, -10.04853567022903782, 2.237415670251142519 ) ) ;
#7843 = ORIENTED_EDGE ( 'NONE', *, *, #1187, .T. ) ;
#7844 = CARTESIAN_POINT ( 'NONE',  ( 15.50000000000000178, -20.99999999999999645, 4.000000000000000000 ) ) ;
#7845 = ORIENTED_EDGE ( 'NONE', *, *, #16549, .F. ) ;
#7846 = CARTESIAN_POINT ( 'NONE',  ( -11.30905858231679595, -23.80360840875935935, 1.768074502826626260 ) ) ;
#7847 = CARTESIAN_POINT ( 'NONE',  ( -22.85856191738413656, 0.000000000000000000, 1.000000000000000000 ) ) ;
#7848 = ADVANCED_FACE ( 'NONE', ( #6488 ), #12850, .F. ) ;
#7849 = CARTESIAN_POINT ( 'NONE',  ( 13.87499999999999467, 5.734882735235988349, 3.999999999999984901 ) ) ;
#7850 = CARTESIAN_POINT ( 'NONE',  ( 1.744064896197293324, -9.868721669903177229, 1.623620860066563365 ) ) ;
#7851 = DIRECTION ( 'NONE',  ( 8.673617379884047798E-17, -1.000000000000000000, 0.000000000000000000 ) ) ;
#7852 = CARTESIAN_POINT ( 'NONE',  ( -13.83770801678722329, 3.866754847752558621, 5.240062463382368030 ) ) ;
#7853 = CARTESIAN_POINT ( 'NONE',  ( 8.309058582316792396, -23.27327832286945153, 2.298404588716537411 ) ) ;
#7854 = CARTESIAN_POINT ( 'NONE',  ( -13.87486364728600208, 4.243114187942282456, 6.725269602253773016 ) ) ;
#7855 = CARTESIAN_POINT ( 'NONE',  ( -27.94203811574922725, 3.231447299068595019E-14, 1.000000000000000000 ) ) ;
#7856 = DIRECTION ( 'NONE',  ( 1.000000000000000000, -0.000000000000000000, -0.000000000000000000 ) ) ;
#7857 = VECTOR ( 'NONE', #3985, 1000.000000000000000 ) ;
#7858 = EDGE_CURVE ( 'NONE', #4979, #7476, #1773, .T. ) ;
#7859 = CARTESIAN_POINT ( 'NONE',  ( 4.940941417683177406, -21.25705176302044208, 2.828734674606458555 ) ) ;
#7860 = CARTESIAN_POINT ( 'NONE',  ( -6.527808582316794173, -23.72900456129165647, 4.275561207030568411 ) ) ;
#7861 = ORIENTED_EDGE ( 'NONE', *, *, #5885, .T. ) ;
#7862 = CARTESIAN_POINT ( 'NONE',  ( 13.37523871602689596, -19.48794484064217514, 4.577160611493482634 ) ) ;
#7863 = PLANE ( 'NONE',  #12003 ) ;
#7864 = ORIENTED_EDGE ( 'NONE', *, *, #14858, .F. ) ;
#7865 = ORIENTED_EDGE ( 'NONE', *, *, #3709, .F. ) ;
#7866 = DIRECTION ( 'NONE',  ( 0.000000000000000000, 0.000000000000000000, 1.000000000000000000 ) ) ;
#7867 = DIRECTION ( 'NONE',  ( -1.000000000000000000, -2.312964634635731617E-15, 0.000000000000000000 ) ) ;
#7868 = ADVANCED_FACE ( 'NONE', ( #6267 ), #18838, .F. ) ;
#7869 = EDGE_CURVE ( 'NONE', #6263, #11591, #13793, .T. ) ;
#7870 = VECTOR ( 'NONE', #4685, 1000.000000000000000 ) ;
#7871 = CARTESIAN_POINT ( 'NONE',  ( -3.211992482548209349, -9.366834950279640637, 2.629956289783360823 ) ) ;
#7872 = LINE ( 'NONE', #6297, #13675 ) ;
#7873 = EDGE_CURVE ( 'NONE', #12771, #1689, #12540, .T. ) ;
#7874 = CARTESIAN_POINT ( 'NONE',  ( 2.682825141213236009, -9.727160171598653093, 1.779880022082258373 ) ) ;
#7875 = CARTESIAN_POINT ( 'NONE',  ( 0.000000000000000000, 4.999999999999999112, 1.000000000000000000 ) ) ;
#7876 = CARTESIAN_POINT ( 'NONE',  ( 11.59030858231679417, -21.32581373872472952, 1.729004561291657138 ) ) ;
#7877 = LINE ( 'NONE', #3071, #12737 ) ;
#7878 = CARTESIAN_POINT ( 'NONE',  ( 12.73577686058281344, -15.40576854059989920, 6.340204579155907183 ) ) ;
#7879 = CARTESIAN_POINT ( 'NONE',  ( -7.371558582316795949, -19.49999999999998934, 3.449312527122348371 ) ) ;
#7880 = CARTESIAN_POINT ( 'NONE',  ( -2.049450250860079592, -10.15122911285664564, 1.696174415070213382 ) ) ;
#7881 = ORIENTED_EDGE ( 'NONE', *, *, #13362, .F. ) ;
#7882 = CARTESIAN_POINT ( 'NONE',  ( -13.84500676459759383, 4.235341612176667603, 5.016097456370799179 ) ) ;
#7883 = DIRECTION ( 'NONE',  ( -0.000000000000000000, -0.000000000000000000, -1.000000000000000000 ) ) ;
#7884 = EDGE_CURVE ( 'NONE', #17458, #12251, #3037, .T. ) ;
#7885 = CARTESIAN_POINT ( 'NONE',  ( 12.53469141768317741, -20.22900456129164581, 2.825813738724747726 ) ) ;
#7886 = CARTESIAN_POINT ( 'NONE',  ( -4.472191417683178294, -22.97900456129165292, 3.035098964749240125 ) ) ;
#7887 = VERTEX_POINT ( 'NONE', #20419 ) ;
#7888 = CARTESIAN_POINT ( 'NONE',  ( 13.45671396861735403, -16.87344458480707843, 6.294109435864141844 ) ) ;
#7889 = DIRECTION ( 'NONE',  ( 0.000000000000000000, 1.000000000000000000, -0.000000000000000000 ) ) ;
#7890 = DIRECTION ( 'NONE',  ( 0.000000000000000000, 0.000000000000000000, -1.000000000000000000 ) ) ;
#7891 = ORIENTED_EDGE ( 'NONE', *, *, #566, .F. ) ;
#7892 = ORIENTED_EDGE ( 'NONE', *, *, #1239, .F. ) ;
#7893 = DIRECTION ( 'NONE',  ( -0.000000000000000000, 0.000000000000000000, -1.000000000000000000 ) ) ;
#7894 = CARTESIAN_POINT ( 'NONE',  ( -22.81633994409548549, 0.000000000000000000, 1.000000000000000000 ) ) ;
#7895 = ORIENTED_EDGE ( 'NONE', *, *, #4493, .F. ) ;
#7896 = CARTESIAN_POINT ( 'NONE',  ( -3.984239023773645805, -21.65718589142769446, 5.016651699346909687 ) ) ;
#7897 = LINE ( 'NONE', #18993, #2001 ) ;
#7898 = DIRECTION ( 'NONE',  ( 1.000000000000000000, 0.000000000000000000, 0.000000000000000000 ) ) ;
#7899 = CARTESIAN_POINT ( 'NONE',  ( 2.226467333542268445, -8.440126719678968215, 1.641959103308203716 ) ) ;
#7900 = CARTESIAN_POINT ( 'NONE',  ( -7.369520639128046113, 9.000000000000001776, 1.000000000000000000 ) ) ;
#7901 = DIRECTION ( 'NONE',  ( 0.000000000000000000, -0.000000000000000000, -1.000000000000000000 ) ) ;
#7902 = CARTESIAN_POINT ( 'NONE',  ( 4.247260319564023945, 0.000000000000000000, 1.000000000000000000 ) ) ;
#7903 = CARTESIAN_POINT ( 'NONE',  ( 3.747260319564023501, 4.999999999999999112, 1.000000000000000000 ) ) ;
#7904 = CARTESIAN_POINT ( 'NONE',  ( -12.71530858231679240, -23.77099543870833998, 2.825813738724734847 ) ) ;
#7905 = CARTESIAN_POINT ( 'NONE',  ( -4.250698171653726654, 16.00000000000000000, 1.000000000000000000 ) ) ;
#7906 = CARTESIAN_POINT ( 'NONE',  ( 5.784691417683178294, -23.02099543870834353, 3.863526089495429972 ) ) ;
#7907 = CARTESIAN_POINT ( 'NONE',  ( -12.62499999999998224, -19.49999999999998934, 4.291666666666699825 ) ) ;
#7908 = CARTESIAN_POINT ( 'NONE',  ( -13.27780858231679595, -20.27099543870833642, 2.724438792969431589 ) ) ;
#7909 = ADVANCED_FACE ( 'NONE', ( #7938, #16303, #10132 ), #11494, .T. ) ;
#7910 = CARTESIAN_POINT ( 'NONE',  ( -3.944195004867014909, -21.42722504787766624, 5.934029185143018914 ) ) ;
#7911 = VERTEX_POINT ( 'NONE', #5116 ) ;
#7912 = CARTESIAN_POINT ( 'NONE',  ( 13.37499999998404299, -19.49999999996810729, 2.793053905886972998 ) ) ;
#7913 = PLANE ( 'NONE',  #3678 ) ;
#7914 = ORIENTED_EDGE ( 'NONE', *, *, #11381, .T. ) ;
#7915 = CARTESIAN_POINT ( 'NONE',  ( -3.500698171653725765, 10.00000000000000000, 1.000000000000000000 ) ) ;
#7916 = VERTEX_POINT ( 'NONE', #19654 ) ;
#7917 = CARTESIAN_POINT ( 'NONE',  ( 0.000000000000000000, 4.999999999999999112, 1.000000000000000000 ) ) ;
#7918 = ORIENTED_EDGE ( 'NONE', *, *, #19649, .T. ) ;
#7919 = CARTESIAN_POINT ( 'NONE',  ( 12.44094141768317741, -20.72672167713052715, 2.298404588716546293 ) ) ;
#7920 = PLANE ( 'NONE',  #2953 ) ;
#7921 = CARTESIAN_POINT ( 'NONE',  ( -1.548630333695928396, -9.114917468222230923, 2.372643865078341019 ) ) ;
#7922 = CARTESIAN_POINT ( 'NONE',  ( 0.000000000000000000, 4.999999999999999112, 1.000000000000000000 ) ) ;
#7923 = CARTESIAN_POINT ( 'NONE',  ( -12.05905858231679417, -20.72672167713054137, 4.701595411283463477 ) ) ;
#7924 = DIRECTION ( 'NONE',  ( 0.000000000000000000, -1.000000000000000000, 0.000000000000000000 ) ) ;
#7925 = CARTESIAN_POINT ( 'NONE',  ( 6.065941417683177406, -23.73192549717336064, 1.696391591240623331 ) ) ;
#7926 = CARTESIAN_POINT ( 'NONE',  ( -12.06594141768317563, -23.20159541128344927, 2.226721677130534705 ) ) ;
#7927 = ORIENTED_EDGE ( 'NONE', *, *, #3614, .T. ) ;
#7928 = CARTESIAN_POINT ( 'NONE',  ( 5.215308582316793284, -23.77099543870833998, 2.825813738724734847 ) ) ;
#7929 = DIRECTION ( 'NONE',  ( 0.000000000000000000, 0.000000000000000000, -1.000000000000000000 ) ) ;
#7930 = CARTESIAN_POINT ( 'NONE',  ( -13.90394305879618386, 5.711624469205903942, 5.287712306078340418 ) ) ;
#7931 = ORIENTED_EDGE ( 'NONE', *, *, #16394, .T. ) ;
#7932 = EDGE_CURVE ( 'NONE', #5732, #19679, #20496, .T. ) ;
#7933 = CARTESIAN_POINT ( 'NONE',  ( 6.715308582316794173, -23.77099543870833998, 2.825813738724734847 ) ) ;
#7934 = DIRECTION ( 'NONE',  ( -0.000000000000000000, -0.000000000000000000, -1.000000000000000000 ) ) ;
#7935 = VERTEX_POINT ( 'NONE', #14621 ) ;
#7936 = LINE ( 'NONE', #12537, #14263 ) ;
#7937 = ORIENTED_EDGE ( 'NONE', *, *, #17975, .F. ) ;
#7938 = FACE_BOUND ( 'NONE', #145, .T. ) ;
#7939 = EDGE_CURVE ( 'NONE', #9894, #17687, #1784, .T. ) ;
#7940 = ORIENTED_EDGE ( 'NONE', *, *, #16763, .F. ) ;
#7941 = CARTESIAN_POINT ( 'NONE',  ( -12.90280858231679595, -23.08622137881038938, 1.020995438708339309 ) ) ;
#7942 = CARTESIAN_POINT ( 'NONE',  ( 12.63249216759192350, -19.87164553660301536, 5.297612231341934041 ) ) ;
#7943 = DIRECTION ( 'NONE',  ( 1.000000000000000000, 0.000000000000000000, 0.000000000000000000 ) ) ;
#7944 = CARTESIAN_POINT ( 'NONE',  ( 1.797685059409938280, -9.880079706704160358, 1.626537830816663588 ) ) ;
#7945 = DIRECTION ( 'NONE',  ( -1.000000000000000000, 4.625929269271486111E-15, 0.000000000000000000 ) ) ;
#7946 = CARTESIAN_POINT ( 'NONE',  ( -13.38210008768272630, -19.14144557202113006, 4.745270796715706396 ) ) ;
#7947 = CARTESIAN_POINT ( 'NONE',  ( 8.777808582316792396, -20.27099543870833642, 2.724438792969431589 ) ) ;
#7948 = CARTESIAN_POINT ( 'NONE',  ( -12.62672826945118665, -20.91272239271162903, 5.058631648758789900 ) ) ;
#7949 = LINE ( 'NONE', #3353, #2034 ) ;
#7950 = CARTESIAN_POINT ( 'NONE',  ( -9.527808582316795949, -24.47900456129166358, 4.586221378810390270 ) ) ;
#7951 = CARTESIAN_POINT ( 'NONE',  ( 8.027808582316792396, -23.72900456129165647, 4.275561207030568411 ) ) ;
#7952 = EDGE_CURVE ( 'NONE', #20223, #18461, #13363, .T. ) ;
#7953 = CARTESIAN_POINT ( 'NONE',  ( 4.847191417683177406, -21.53509896474923835, 2.520995438708346192 ) ) ;
#7954 = CARTESIAN_POINT ( 'NONE',  ( -10.28469141768317741, -23.77099543870834353, 4.174186261275251830 ) ) ;
#7955 = STYLED_ITEM ( 'NONE', ( #394 ), #18044 ) ;
#7956 = VERTEX_POINT ( 'NONE', #201 ) ;
#7957 = CARTESIAN_POINT ( 'NONE',  ( 13.84501469867711698, 4.235742283194553259, 4.666666666666618113 ) ) ;
#7958 = CARTESIAN_POINT ( 'NONE',  ( -14.49999999999998579, -19.49999999999999645, 4.000000000000000000 ) ) ;
#7959 = AXIS2_PLACEMENT_3D ( 'NONE', #12218, #4484, #5943 ) ;
#7960 = EDGE_LOOP ( 'NONE', ( #10674, #8381, #9173, #14159, #13876, #11131, #15164, #4500 ) ) ;
#7961 = PRODUCT_DEFINITION_CONTEXT ( 'detailed design', #18706, 'design' ) ;
#7962 = ORIENTED_EDGE ( 'NONE', *, *, #6444, .F. ) ;
#7963 = CARTESIAN_POINT ( 'NONE',  ( 29.71062960567705602, 11.64110105645932691, 0.000000000000000000 ) ) ;
#7964 = DIRECTION ( 'NONE',  ( 0.000000000000000000, 0.000000000000000000, -1.000000000000000000 ) ) ;
#7965 = CARTESIAN_POINT ( 'NONE',  ( -13.12463908936614132, 4.981774012991869505, 5.264611377988129171 ) ) ;
#7966 = VECTOR ( 'NONE', #7157, 1000.000000000000000 ) ;
#7967 = VECTOR ( 'NONE', #18402, 1000.000000000000000 ) ;
#7968 = CARTESIAN_POINT ( 'NONE',  ( -1.513434189748285696, -9.114917468222230923, 2.372643865078341019 ) ) ;
#7969 = DIRECTION ( 'NONE',  ( -1.000000000000000000, 0.000000000000000000, 0.000000000000000000 ) ) ;
#7970 = VECTOR ( 'NONE', #11148, 1000.000000000000000 ) ;
#7971 = CARTESIAN_POINT ( 'NONE',  ( 14.50000000000001243, -25.49999999999999645, 4.000000000000000000 ) ) ;
#7972 = CARTESIAN_POINT ( 'NONE',  ( -13.08094078691552831, 2.775009739235173356, 5.981149842915306714 ) ) ;
#7973 = CARTESIAN_POINT ( 'NONE',  ( 9.996558582316794173, -22.05068747287764452, 1.749999999999998446 ) ) ;
#7974 = PLANE ( 'NONE',  #9079 ) ;
#7975 = CARTESIAN_POINT ( 'NONE',  ( 12.75496035233418013, -14.43700220713569138, 6.361037912489419632 ) ) ;
#7976 = CARTESIAN_POINT ( 'NONE',  ( -1.866357130655357688, -10.00562759449716133, 2.408781036472938730 ) ) ;
#7977 = ORIENTED_EDGE ( 'NONE', *, *, #7540, .F. ) ;
#7978 = CARTESIAN_POINT ( 'NONE',  ( -13.40382044110196347, -18.79456772435387890, 5.502763032956559108 ) ) ;
#7979 = CARTESIAN_POINT ( 'NONE',  ( 27.44203811574919882, 10.00000000000000000, 0.000000000000000000 ) ) ;
#7980 = EDGE_CURVE ( 'NONE', #1638, #1689, #3646, .T. ) ;
#7981 = CARTESIAN_POINT ( 'NONE',  ( 7.847191417683175629, -20.91377862118959285, 1.020995438708345082 ) ) ;
#7982 = CARTESIAN_POINT ( 'NONE',  ( -11.68405858231679595, -21.32873467460644079, 2.757051763020455404 ) ) ;
#7983 = ORIENTED_EDGE ( 'NONE', *, *, #9887, .T. ) ;
#7984 = ADVANCED_FACE ( 'NONE', ( #5317 ), #3544, .T. ) ;
#7985 = AXIS2_PLACEMENT_3D ( 'NONE', #7421, #9088, #18292 ) ;
#7986 = CARTESIAN_POINT ( 'NONE',  ( 13.89075858682503650, 5.045808634669852744, 6.406973581600956535 ) ) ;
#7987 = CARTESIAN_POINT ( 'NONE',  ( 13.09892531043291086, 3.683228176858501790, 6.000681092915118420 ) ) ;
#7988 = VECTOR ( 'NONE', #17511, 1000.000000000000000 ) ;
#7989 = FACE_OUTER_BOUND ( 'NONE', #19918, .T. ) ;
#7990 = ORIENTED_EDGE ( 'NONE', *, *, #15577, .T. ) ;
#7991 = CIRCLE ( 'NONE', #1648, 0.3750000000000003331 ) ;
#7992 = EDGE_LOOP ( 'NONE', ( #19405, #2545, #1114, #6710 ) ) ;
#7993 = DIRECTION ( 'NONE',  ( -0.000000000000000000, -0.000000000000000000, -1.000000000000000000 ) ) ;
#7994 = VECTOR ( 'NONE', #8752, 1000.000000000000000 ) ;
#7995 = DIRECTION ( 'NONE',  ( 0.000000000000000000, 0.000000000000000000, 1.000000000000000000 ) ) ;
#7996 = FACE_OUTER_BOUND ( 'NONE', #13103, .T. ) ;
#7997 = EDGE_CURVE ( 'NONE', #8562, #13563, #1643, .T. ) ;
#7998 = CARTESIAN_POINT ( 'NONE',  ( 4.000698171653723101, 0.000000000000000000, 1.000000000000000000 ) ) ;
#7999 = CARTESIAN_POINT ( 'NONE',  ( -3.499999999999998668, -19.50000000000000000, 1.000000000000000000 ) ) ;
#8000 = CARTESIAN_POINT ( 'NONE',  ( 2.442511739767545098, -14.09457879449248807, 3.458905389639174821 ) ) ;
#8001 = CARTESIAN_POINT ( 'NONE',  ( 0.000000000000000000, 9.000000000000001776, 0.000000000000000000 ) ) ;
#8002 = DIRECTION ( 'NONE',  ( 0.000000000000000000, 1.000000000000000000, 0.000000000000000000 ) ) ;
#8003 = DIRECTION ( 'NONE',  ( 0.000000000000000000, 0.000000000000000000, 1.000000000000000000 ) ) ;
#8004 = AXIS2_PLACEMENT_3D ( 'NONE', #19817, #13820, #4311 ) ;
#8005 = FACE_OUTER_BOUND ( 'NONE', #9863, .T. ) ;
#8006 = CARTESIAN_POINT ( 'NONE',  ( -12.05905858231679417, -20.72672167713054137, 4.701595411283463477 ) ) ;
#8007 = CARTESIAN_POINT ( 'NONE',  ( -1.743623630681728542, -9.116095536440919744, 2.372946416531167557 ) ) ;
#8008 = CARTESIAN_POINT ( 'NONE',  ( 11.21530858231679595, -23.02099543870833998, 3.136473910504556262 ) ) ;
#8009 = CARTESIAN_POINT ( 'NONE',  ( -12.62868952012632207, -19.31367923361656480, 4.748088538831167327 ) ) ;
#8010 = CARTESIAN_POINT ( 'NONE',  ( -5.965308582316795949, -20.97900456129165647, 3.863526089495444626 ) ) ;
#8011 = AXIS2_PLACEMENT_3D ( 'NONE', #4171, #2596, #8784 ) ;
#8012 = EDGE_CURVE ( 'NONE', #13542, #13028, #17604, .T. ) ;
#8013 = CARTESIAN_POINT ( 'NONE',  ( -3.974842109207560537, -21.73478823434188456, 6.006404853634143670 ) ) ;
#8014 = ORIENTED_EDGE ( 'NONE', *, *, #6856, .F. ) ;
#8015 = EDGE_CURVE ( 'NONE', #3751, #11612, #4550, .T. ) ;
#8016 = CARTESIAN_POINT ( 'NONE',  ( 13.37500000000002132, -19.49999999999450040, 3.833333333368183382 ) ) ;
#8017 = CARTESIAN_POINT ( 'NONE',  ( -9.805650798910056309, 4.999999999999999112, 1.000000000000000000 ) ) ;
#8018 = EDGE_LOOP ( 'NONE', ( #17769, #3324, #18934, #10828, #6193, #4235, #14439, #5907 ) ) ;
#8019 = VERTEX_POINT ( 'NONE', #12285 ) ;
#8020 = DIRECTION ( 'NONE',  ( -0.000000000000000000, 0.000000000000000000, -1.000000000000000000 ) ) ;
#8021 = CARTESIAN_POINT ( 'NONE',  ( 13.86436316834274329, 3.712840001305938831, 6.736817769197426031 ) ) ;
#8022 = ORIENTED_EDGE ( 'NONE', *, *, #6560, .F. ) ;
#8023 = DIRECTION ( 'NONE',  ( 3.469446951953619119E-16, 1.000000000000000000, -0.000000000000000000 ) ) ;
#8024 = AXIS2_PLACEMENT_3D ( 'NONE', #4834, #3265, #8086 ) ;
#8025 = PRESENTATION_LAYER_ASSIGNMENT (  '', '', ( #20054 ) ) ;
#8026 = ORIENTED_EDGE ( 'NONE', *, *, #10465, .T. ) ;
#8027 = COLOUR_RGB ( '', 0.66274510, 0.83137255, 0.94901961) ;
#8028 = CARTESIAN_POINT ( 'NONE',  ( 10.84719141768317741, -21.22443879296941915, 1.770995438708345748 ) ) ;
#8029 = EDGE_CURVE ( 'NONE', #14610, #381, #18613, .T. ) ;
#8030 = DIRECTION ( 'NONE',  ( 1.000000000000000000, 0.000000000000000000, -0.000000000000000000 ) ) ;
#8031 = AXIS2_PLACEMENT_3D ( 'NONE', #1587, #19178, #3260 ) ;
#8032 = CARTESIAN_POINT ( 'NONE',  ( -2.817596665886821672, -11.50588678273290988, 2.986692549455723267 ) ) ;
#8033 = DIRECTION ( 'NONE',  ( 1.000000000000000000, 0.000000000000000000, -0.000000000000000000 ) ) ;
#8034 = CARTESIAN_POINT ( 'NONE',  ( -11.49655858231679417, -22.05068747287764452, 1.749999999999998446 ) ) ;
#8035 = SURFACE_STYLE_FILL_AREA ( #185 ) ;
#8036 = VECTOR ( 'NONE', #11901, 1000.000000000000000 ) ;
#8037 = CARTESIAN_POINT ( 'NONE',  ( 5.597191417683177406, -23.08622137881040359, 5.979004561291654696 ) ) ;
#8038 = DIRECTION ( 'NONE',  ( 1.000000000000000000, 0.000000000000000000, 0.000000000000000000 ) ) ;
#8039 = CARTESIAN_POINT ( 'NONE',  ( -5.503441417683176518, -22.05068747287765873, 5.250000000000000888 ) ) ;
#8040 = AXIS2_PLACEMENT_3D ( 'NONE', #2610, #18626, #19792 ) ;
#8041 = VERTEX_POINT ( 'NONE', #1212 ) ;
#8042 = CARTESIAN_POINT ( 'NONE',  ( 4.687312169500632564, -21.51559725698341197, 5.182386163300427562 ) ) ;
#8043 = CARTESIAN_POINT ( 'NONE',  ( 13.49999999999998401, -18.49999999999999645, 4.000000000000000000 ) ) ;
#8044 = CARTESIAN_POINT ( 'NONE',  ( -12.62499963760179256, -21.00001830110826972, 4.442557003548452066 ) ) ;
#8045 = VECTOR ( 'NONE', #15588, 1000.000000000000000 ) ;
#8046 = VERTEX_POINT ( 'NONE', #7588 ) ;
#8047 = AXIS2_PLACEMENT_3D ( 'NONE', #18367, #3821, #4231 ) ;
#8048 = VECTOR ( 'NONE', #15330, 1000.000000000000000 ) ;
#8049 = CARTESIAN_POINT ( 'NONE',  ( 5.965308582316793284, -20.22900456129164937, 4.174186261275266929 ) ) ;
#8050 = CARTESIAN_POINT ( 'NONE',  ( -4.999999999999997335, -7.500000000000000000, 1.000000000000000000 ) ) ;
#8051 = ORIENTED_EDGE ( 'NONE', *, *, #4274, .T. ) ;
#8052 = DIRECTION ( 'NONE',  ( -1.000000000000000000, 0.000000000000000000, 0.000000000000000000 ) ) ;
#8053 = CARTESIAN_POINT ( 'NONE',  ( 0.000000000000000000, 0.000000000000000000, 0.000000000000000000 ) ) ;
#8054 = ORIENTED_EDGE ( 'NONE', *, *, #4678, .F. ) ;
#8055 = CARTESIAN_POINT ( 'NONE',  ( -14.49999999999998579, -25.49999999999999645, 4.000000000000000000 ) ) ;
#8056 = EDGE_LOOP ( 'NONE', ( #6401, #6458, #18053, #11581 ) ) ;
#8057 = CARTESIAN_POINT ( 'NONE',  ( -6.621558582316794173, -23.74999999999999645, 3.550687472877651629 ) ) ;
#8058 = CARTESIAN_POINT ( 'NONE',  ( 12.62500000000001954, -20.24999999999506173, 3.850307403176420618 ) ) ;
#8059 = CIRCLE ( 'NONE', #13390, 2.999999999999999112 ) ;
#8060 = PLANE ( 'NONE',  #14811 ) ;
#8061 = CARTESIAN_POINT ( 'NONE',  ( 1.548630333695928396, -9.114917468222230923, 1.622643865078341463 ) ) ;
#8062 = VECTOR ( 'NONE', #19717, 1000.000000000000000 ) ;
#8063 = EDGE_CURVE ( 'NONE', #7740, #6147, #2879, .T. ) ;
#8064 = AXIS2_PLACEMENT_3D ( 'NONE', #16969, #2857, #2646 ) ;
#8065 = CARTESIAN_POINT ( 'NONE',  ( 0.000000000000000000, 4.999999999999999112, 0.000000000000000000 ) ) ;
#8066 = CARTESIAN_POINT ( 'NONE',  ( -13.41806913471718588, -17.32500869677464550, 4.784333296715663764 ) ) ;
#8067 = CARTESIAN_POINT ( 'NONE',  ( 6.434058582316794173, -23.20159541128345992, 4.773278322869455970 ) ) ;
#8068 = CARTESIAN_POINT ( 'NONE',  ( -12.62499999998404299, -20.99999999996810729, 2.793053905886972998 ) ) ;
#8069 = CARTESIAN_POINT ( 'NONE',  ( 17.12779268661489596, 11.64110105645932691, 0.000000000000000000 ) ) ;
#8070 = CARTESIAN_POINT ( 'NONE',  ( -11.02780858231679595, -24.47900456129166358, 4.586221378810390270 ) ) ;
#8071 = CARTESIAN_POINT ( 'NONE',  ( 5.871558582316794173, -20.24999999999999289, 3.449312527122348371 ) ) ;
#8072 = CARTESIAN_POINT ( 'NONE',  ( 7.284691417683176518, -23.02099543870834353, 3.863526089495429972 ) ) ;
#8073 = CARTESIAN_POINT ( 'NONE',  ( -8.128441417683175629, -20.24999999999999289, 3.550687472877664952 ) ) ;
#8074 = VERTEX_POINT ( 'NONE', #12590 ) ;
#8075 = ORIENTED_EDGE ( 'NONE', *, *, #20385, .T. ) ;
#8076 = CARTESIAN_POINT ( 'NONE',  ( 13.84500676459759383, 4.235341612176667603, 5.016097456370799179 ) ) ;
#8077 = DIRECTION ( 'NONE',  ( -0.000000000000000000, -0.000000000000000000, -1.000000000000000000 ) ) ;
#8078 = LINE ( 'NONE', #8384, #1341 ) ;
#8079 = ORIENTED_EDGE ( 'NONE', *, *, #281, .F. ) ;
#8080 = AXIS2_PLACEMENT_3D ( 'NONE', #18204, #16611, #736 ) ;
#8081 = ORIENTED_EDGE ( 'NONE', *, *, #14525, .F. ) ;
#8082 = CARTESIAN_POINT ( 'NONE',  ( 0.6250000000000005551, 11.64110105645932691, 0.000000000000000000 ) ) ;
#8083 = CARTESIAN_POINT ( 'NONE',  ( 17.11324865405191176, -10.99999999999999645, 2.000000000000000000 ) ) ;
#8084 = CARTESIAN_POINT ( 'NONE',  ( -13.10756170493883310, 4.119366099410778581, 6.001761809183453700 ) ) ;
#8085 = CARTESIAN_POINT ( 'NONE',  ( -2.445888733774860935, -8.532121313016713060, 2.415585152653916712 ) ) ;
#8086 = DIRECTION ( 'NONE',  ( 0.000000000000000000, -0.000000000000000000, 1.000000000000000000 ) ) ;
#8087 = ADVANCED_FACE ( 'NONE', ( #719 ), #12392, .T. ) ;
#8088 = DIRECTION ( 'NONE',  ( -1.156482317317871133E-15, -1.000000000000000000, 0.000000000000000000 ) ) ;
#8089 = CARTESIAN_POINT ( 'NONE',  ( -12.91308523408712183, -5.701695678577235249, 5.798858176249892082 ) ) ;
#8090 = CARTESIAN_POINT ( 'NONE',  ( 12.99655858231679417, -22.05068747287764452, 1.749999999999998446 ) ) ;
#8091 = DIRECTION ( 'NONE',  ( -1.000000000000000000, 0.000000000000000000, 0.000000000000000000 ) ) ;
#8092 = CARTESIAN_POINT ( 'NONE',  ( 13.11345185444515415, 3.666818649476655700, 6.750360829155977349 ) ) ;
#8093 = VECTOR ( 'NONE', #9708, 1000.000000000000000 ) ;
#8094 = CARTESIAN_POINT ( 'NONE',  ( -1.963707630584672570, -9.980492102769451535, 1.652325740065381909 ) ) ;
#8095 = ADVANCED_FACE ( 'NONE', ( #17410 ), #17202, .T. ) ;
#8096 = ORIENTED_EDGE ( 'NONE', *, *, #9361, .T. ) ;
#8097 = EDGE_CURVE ( 'NONE', #2482, #7326, #7103, .T. ) ;
#8098 = CARTESIAN_POINT ( 'NONE',  ( -13.47096266223369376, -15.40388555723029462, 5.575679699623145247 ) ) ;
#8099 = CARTESIAN_POINT ( 'NONE',  ( -0.000000000000000000, 10.00000000000000000, 0.000000000000000000 ) ) ;
#8100 = CARTESIAN_POINT ( 'NONE',  ( 4.190941417683176518, -23.80360840875937001, 5.231925497173365081 ) ) ;
#8101 = CARTESIAN_POINT ( 'NONE',  ( -9.340308582316795949, -22.36352608949544418, 4.520995438708343528 ) ) ;
#8102 = ORIENTED_EDGE ( 'NONE', *, *, #3407, .T. ) ;
#8103 = CARTESIAN_POINT ( 'NONE',  ( 13.86833701876684088, 3.913519447696059750, 6.741146579470268740 ) ) ;
#8104 = CARTESIAN_POINT ( 'NONE',  ( 13.12119116326504908, 4.807653744879115010, 5.626470997801169105 ) ) ;
#8105 = DIRECTION ( 'NONE',  ( 0.000000000000000000, -0.000000000000000000, 1.000000000000000000 ) ) ;
#8106 = EDGE_LOOP ( 'NONE', ( #18299, #15927, #13324, #7794 ) ) ;
#8107 = EDGE_LOOP ( 'NONE', ( #12768, #20207, #16906, #6071 ) ) ;
#8108 = LINE ( 'NONE', #17506, #2422 ) ;
#8109 = CARTESIAN_POINT ( 'NONE',  ( 0.000000000000000000, 10.00000000000000000, 1.000000000000000000 ) ) ;
#8110 = CARTESIAN_POINT ( 'NONE',  ( -13.81494360078803396, 0.000000000000000000, 0.000000000000000000 ) ) ;
#8111 = EDGE_CURVE ( 'NONE', #8663, #16909, #3514, .T. ) ;
#8112 = DIRECTION ( 'NONE',  ( 1.000000000000000000, 0.000000000000000000, -0.000000000000000000 ) ) ;
#8113 = CARTESIAN_POINT ( 'NONE',  ( 1.925499516411631973, -10.42380411186744382, 2.516177120048874283 ) ) ;
#8114 = DIRECTION ( 'NONE',  ( -0.000000000000000000, -0.000000000000000000, -1.000000000000000000 ) ) ;
#8115 = DIRECTION ( 'NONE',  ( 0.000000000000000000, 0.000000000000000000, -1.000000000000000000 ) ) ;
#8116 = CARTESIAN_POINT ( 'NONE',  ( 20.49999999999998224, -21.99999999999999645, 12.00000000000000355 ) ) ;
#8117 = CARTESIAN_POINT ( 'NONE',  ( -13.67791111847408025, 0.000000000000000000, 1.000000000000000000 ) ) ;
#8118 = CARTESIAN_POINT ( 'NONE',  ( -11.21530858231679417, -23.77099543870833998, 2.825813738724734847 ) ) ;
#8119 = CARTESIAN_POINT ( 'NONE',  ( -1.337453470010121714, -9.114917468222230923, 2.372643865078341019 ) ) ;
#8120 = CARTESIAN_POINT ( 'NONE',  ( 8.121558582316795949, -22.99999999999999645, 3.550687472877652073 ) ) ;
#8121 = CARTESIAN_POINT ( 'NONE',  ( -12.62499999999998224, -19.50000000000006040, 4.416666666666682062 ) ) ;
#8122 = CARTESIAN_POINT ( 'NONE',  ( -10.93405858231679417, -23.20159541128345992, 4.773278322869455970 ) ) ;
#8123 = VECTOR ( 'NONE', #12364, 1000.000000000000000 ) ;
#8124 = CARTESIAN_POINT ( 'NONE',  ( -6.909691417683176518, -21.01515356694492098, 6.020995438708349745 ) ) ;
#8125 = ORIENTED_EDGE ( 'NONE', *, *, #17284, .T. ) ;
#8126 = CARTESIAN_POINT ( 'NONE',  ( 13.83411111208379474, 3.685111160228107252, 5.236156213382356484 ) ) ;
#8127 = CARTESIAN_POINT ( 'NONE',  ( -20.00000000000000000, 2.499999999999999556, 1.500000000000000000 ) ) ;
#8128 = ORIENTED_EDGE ( 'NONE', *, *, #7346, .T. ) ;
#8129 = EDGE_CURVE ( 'NONE', #13158, #13679, #10618, .T. ) ;
#8130 = ORIENTED_EDGE ( 'NONE', *, *, #10257, .F. ) ;
#8131 = FACE_OUTER_BOUND ( 'NONE', #13954, .T. ) ;
#8132 = ORIENTED_EDGE ( 'NONE', *, *, #16852, .F. ) ;
#8133 = FACE_OUTER_BOUND ( 'NONE', #11665, .T. ) ;
#8134 = AXIS2_PLACEMENT_3D ( 'NONE', #14839, #16602, #16824 ) ;
#8135 = VERTEX_POINT ( 'NONE', #3394 ) ;
#8136 = LINE ( 'NONE', #17439, #17337 ) ;
#8137 = VECTOR ( 'NONE', #18938, 1000.000000000000000 ) ;
#8138 = CARTESIAN_POINT ( 'NONE',  ( -29.18266749954690553, 14.63532295040229059, 0.3390567389149233835 ) ) ;
#8139 = EDGE_CURVE ( 'NONE', #12892, #12897, #11445, .T. ) ;
#8140 = ADVANCED_FACE ( 'NONE', ( #5164 ), #11544, .T. ) ;
#8141 = CARTESIAN_POINT ( 'NONE',  ( -1.513434189748285696, -9.114917468222230923, 2.372643865078341019 ) ) ;
#8142 = CARTESIAN_POINT ( 'NONE',  ( 2.594671182134835163, -9.923034775318452461, 2.580184533305832861 ) ) ;
#8143 = CARTESIAN_POINT ( 'NONE',  ( -12.43405858231679417, -23.20159541128345992, 4.773278322869455970 ) ) ;
#8144 = LINE ( 'NONE', #16088, #14626 ) ;
#8145 = CARTESIAN_POINT ( 'NONE',  ( 11.31594141768317741, -20.79840458871654363, 4.773278322869464851 ) ) ;
#8146 = CARTESIAN_POINT ( 'NONE',  ( 27.49999999999999645, -4.770489558936219510E-14, 1.000000000000000000 ) ) ;
#8147 = CARTESIAN_POINT ( 'NONE',  ( -6.347191417683176518, -21.22443879296941915, 1.770995438708345748 ) ) ;
#8148 = VECTOR ( 'NONE', #7277, 1000.000000000000000 ) ;
#8149 = ORIENTED_EDGE ( 'NONE', *, *, #13568, .F. ) ;
#8150 = CARTESIAN_POINT ( 'NONE',  ( 9.715308582316795949, -24.52099543870834708, 2.515153566944913432 ) ) ;
#8151 = CARTESIAN_POINT ( 'NONE',  ( 12.62499999999998224, -20.24999999999998934, 4.291666666666698937 ) ) ;
#8152 = CARTESIAN_POINT ( 'NONE',  ( -13.15498530132288479, 5.764257716805535559, 4.833333333333343695 ) ) ;
#8153 = ORIENTED_EDGE ( 'NONE', *, *, #1822, .F. ) ;
#8154 = EDGE_CURVE ( 'NONE', #12948, #2020, #16051, .T. ) ;
#8155 = CARTESIAN_POINT ( 'NONE',  ( 13.00209451496117374, 0.000000000000000000, 0.000000000000000000 ) ) ;
#8156 = PLANE ( 'NONE',  #12331 ) ;
#8157 = VERTEX_POINT ( 'NONE', #360 ) ;
#8158 = ORIENTED_EDGE ( 'NONE', *, *, #118, .T. ) ;
#8159 = CARTESIAN_POINT ( 'NONE',  ( 0.000000000000000000, 9.000000000000001776, 1.000000000000000000 ) ) ;
#8160 = VECTOR ( 'NONE', #11953, 1000.000000000000000 ) ;
#8161 = ORIENTED_EDGE ( 'NONE', *, *, #14609, .F. ) ;
#8162 = CARTESIAN_POINT ( 'NONE',  ( -5.027808582316793284, -23.72900456129165647, 4.275561207030568411 ) ) ;
#8163 = CARTESIAN_POINT ( 'NONE',  ( -10.49999999999999822, -9.999999999999992895, 2.000000000000000000 ) ) ;
#8164 = FACE_OUTER_BOUND ( 'NONE', #15785, .T. ) ;
#8165 = CARTESIAN_POINT ( 'NONE',  ( 2.044552395631970665, -10.13052631352519306, 1.690857522621936226 ) ) ;
#8166 = CARTESIAN_POINT ( 'NONE',  ( 13.15498530132288479, 5.764257716805535559, 4.791666666666684726 ) ) ;
#8167 = CYLINDRICAL_SURFACE ( 'NONE', #6689, 2.500000000000000444 ) ;
#8168 = CARTESIAN_POINT ( 'NONE',  ( -13.84167967300649238, 4.067323486828401613, 5.231641758301140754 ) ) ;
#8169 = CARTESIAN_POINT ( 'NONE',  ( 9.340308582316795949, -22.98484643305508612, 6.020995438708344416 ) ) ;
#8170 = CARTESIAN_POINT ( 'NONE',  ( -13.11824772738305356, 3.909010232842670796, 6.755569162489314827 ) ) ;
#8171 = PLANE ( 'NONE',  #3727 ) ;
#8172 = CARTESIAN_POINT ( 'NONE',  ( 8.965308582316794173, -20.22900456129164937, 4.174186261275266929 ) ) ;
#8173 = EDGE_CURVE ( 'NONE', #962, #8046, #19201, .T. ) ;
#8174 = CARTESIAN_POINT ( 'NONE',  ( 7.003441417683177406, -22.05068747287766229, 4.499999999999999112 ) ) ;
#8175 = CARTESIAN_POINT ( 'NONE',  ( -7.097191417683177406, -22.77556120703057729, 5.229004561291656472 ) ) ;
#8176 = ORIENTED_EDGE ( 'NONE', *, *, #20498, .F. ) ;
#8177 = ORIENTED_EDGE ( 'NONE', *, *, #8012, .F. ) ;
#8178 = CARTESIAN_POINT ( 'NONE',  ( 13.37500015856764435, -20.24999199233421265, 4.532157119432948633 ) ) ;
#8179 = CARTESIAN_POINT ( 'NONE',  ( 14.50000000000001243, -18.49999999999999645, 4.000000000000000000 ) ) ;
#8180 = DIRECTION ( 'NONE',  ( 1.000000000000000000, 0.000000000000000000, 0.000000000000000000 ) ) ;
#8181 = VERTEX_POINT ( 'NONE', #4855 ) ;
#8182 = ORIENTED_EDGE ( 'NONE', *, *, #9182, .F. ) ;
#8183 = CARTESIAN_POINT ( 'NONE',  ( -18.98630159782011262, 0.000000000000000000, 1.000000000000000000 ) ) ;
#8184 = CARTESIAN_POINT ( 'NONE',  ( 0.000000000000000000, 0.000000000000000000, 2.000000000000000000 ) ) ;
#8185 = DIRECTION ( 'NONE',  ( 0.000000000000000000, 0.000000000000000000, 1.000000000000000000 ) ) ;
#8186 = CARTESIAN_POINT ( 'NONE',  ( -1.407845757905374695, -8.364917468222230923, 1.622643865078341907 ) ) ;
#8187 = PLANE ( 'NONE',  #20050 ) ;
#8188 = CARTESIAN_POINT ( 'NONE',  ( 0.000000000000000000, 0.000000000000000000, 1.000000000000000000 ) ) ;
#8189 = AXIS2_PLACEMENT_3D ( 'NONE', #14862, #8905, #13396 ) ;
#8190 = CARTESIAN_POINT ( 'NONE',  ( -12.65051119073526564, -18.96168486786632457, 5.513701926248478102 ) ) ;
#8191 = CARTESIAN_POINT ( 'NONE',  ( 8.121558582316792396, -23.74999999999999645, 3.550687472877651629 ) ) ;
#8192 = LINE ( 'NONE', #1496, #5399 ) ;
#8193 = CARTESIAN_POINT ( 'NONE',  ( 13.15498530131898214, 5.764257716805535559, 3.333333333333075466 ) ) ;
#8194 = CARTESIAN_POINT ( 'NONE',  ( -1.859341899742023463, -9.902476528685241419, 1.632289782122827271 ) ) ;
#8195 = VERTEX_POINT ( 'NONE', #9667 ) ;
#8196 = CARTESIAN_POINT ( 'NONE',  ( -13.41341218697771609, -18.31018455762212227, 5.513179699623425023 ) ) ;
#8197 = LINE ( 'NONE', #12995, #2712 ) ;
#8198 = AXIS2_PLACEMENT_3D ( 'NONE', #11342, #9567, #4760 ) ;
#8199 = CARTESIAN_POINT ( 'NONE',  ( 6.722191417683176518, -19.52099543870834353, 4.586221378810406257 ) ) ;
#8200 = CARTESIAN_POINT ( 'NONE',  ( -7.277808582316795061, -21.02099543870833998, 3.035098964749253003 ) ) ;
#8201 = ORIENTED_EDGE ( 'NONE', *, *, #4382, .F. ) ;
#8202 = CARTESIAN_POINT ( 'NONE',  ( 12.62499999999998224, -20.99999999999991829, 4.333333333333343695 ) ) ;
#8203 = CARTESIAN_POINT ( 'NONE',  ( 13.12526104302547836, 5.013182672784613381, 5.066812735559260261 ) ) ;
#8204 = CARTESIAN_POINT ( 'NONE',  ( 3.999999999999999112, -2.500000000000047518, 9.999999999999998224 ) ) ;
#8205 = ORIENTED_EDGE ( 'NONE', *, *, #3529, .T. ) ;
#8206 = ADVANCED_FACE ( 'NONE', ( #17613 ), #9872, .T. ) ;
#8207 = ORIENTED_EDGE ( 'NONE', *, *, #7052, .F. ) ;
#8208 = CARTESIAN_POINT ( 'NONE',  ( 17.80017143803810242, 9.000000000000001776, 1.000000000000000000 ) ) ;
#8209 = DIRECTION ( 'NONE',  ( 1.000000000000000000, 0.000000000000000000, 0.000000000000000000 ) ) ;
#8210 = ADVANCED_FACE ( 'NONE', ( #6637 ), #5068, .T. ) ;
#8211 = EDGE_CURVE ( 'NONE', #13178, #17919, #15907, .T. ) ;
#8212 = EDGE_LOOP ( 'NONE', ( #14420, #16231, #13565, #9154 ) ) ;
#8213 = FACE_OUTER_BOUND ( 'NONE', #11409, .T. ) ;
#8214 = CARTESIAN_POINT ( 'NONE',  ( 0.9854920305337621089, -9.114917468222230923, 1.622643865078341463 ) ) ;
#8215 = DIRECTION ( 'NONE',  ( 0.000000000000000000, 0.000000000000000000, -1.000000000000000000 ) ) ;
#8216 = CARTESIAN_POINT ( 'NONE',  ( -4.000000000000000000, -12.50000000000000000, 3.464723819589916154 ) ) ;
#8217 = DIRECTION ( 'NONE',  ( 1.000000000000000000, 0.000000000000000000, 0.000000000000000000 ) ) ;
#8218 = DIRECTION ( 'NONE',  ( 0.000000000000000000, -1.000000000000000000, 0.000000000000000000 ) ) ;
#8219 = DIRECTION ( 'NONE',  ( -0.1351665943404306014, -0.9596796555888911229, 0.2464649070825229160 ) ) ;
#8220 = CARTESIAN_POINT ( 'NONE',  ( -2.702705060698113115, -10.69015907548275379, 2.777197378435510622 ) ) ;
#8221 = ORIENTED_EDGE ( 'NONE', *, *, #10000, .T. ) ;
#8222 = CARTESIAN_POINT ( 'NONE',  ( -12.62933427970994238, -19.28111887465110996, 4.754790882998214840 ) ) ;
#8223 = CARTESIAN_POINT ( 'NONE',  ( -11.21530858231679417, -23.77099543870833998, 2.825813738724734847 ) ) ;
#8224 = CARTESIAN_POINT ( 'NONE',  ( -4.472191417683177406, -23.72900456129165292, 2.724438792969417822 ) ) ;
#8225 = VERTEX_POINT ( 'NONE', #3494 ) ;
#8226 = CARTESIAN_POINT ( 'NONE',  ( 13.84090061271218985, 4.027980941966571748, 5.240332426532912535 ) ) ;
#8227 = LINE ( 'NONE', #13027, #2697 ) ;
#8228 = VERTEX_POINT ( 'NONE', #13009 ) ;
#8229 = ORIENTED_EDGE ( 'NONE', *, *, #19634, .T. ) ;
#8230 = CARTESIAN_POINT ( 'NONE',  ( 20.00000000000000000, -5.999999999999994671, 1.000000000000000000 ) ) ;
#8231 = EDGE_CURVE ( 'NONE', #17224, #10279, #14574, .T. ) ;
#8232 = ORIENTED_EDGE ( 'NONE', *, *, #10118, .T. ) ;
#8233 = DIRECTION ( 'NONE',  ( 0.000000000000000000, 1.000000000000000000, -0.000000000000000000 ) ) ;
#8234 = VECTOR ( 'NONE', #942, 1000.000000000000000 ) ;
#8235 = ORIENTED_EDGE ( 'NONE', *, *, #1510, .T. ) ;
#8236 = CARTESIAN_POINT ( 'NONE',  ( 8.784691417683177406, -23.77099543870834353, 4.174186261275251830 ) ) ;
#8237 = CARTESIAN_POINT ( 'NONE',  ( -11.00000000000000000, -20.29006350946107418, 5.466506350946110260 ) ) ;
#8238 = CARTESIAN_POINT ( 'NONE',  ( -2.659620708751979645, -10.38426118526329489, 2.698636689302993830 ) ) ;
#8239 = DIRECTION ( 'NONE',  ( -0.000000000000000000, 0.000000000000000000, -1.000000000000000000 ) ) ;
#8240 = CARTESIAN_POINT ( 'NONE',  ( -10.84030858231679240, -22.67418626127525982, 5.270995438708342640 ) ) ;
#8241 = CARTESIAN_POINT ( 'NONE',  ( 10.94094141768317741, -20.72672167713052715, 2.298404588716546293 ) ) ;
#8242 = DIRECTION ( 'NONE',  ( 0.000000000000000000, 0.000000000000000000, -1.000000000000000000 ) ) ;
#8243 = CARTESIAN_POINT ( 'NONE',  ( -5.222191417683178294, -20.27099543870833998, 4.275561207030583510 ) ) ;
#8244 = VERTEX_POINT ( 'NONE', #17507 ) ;
#8245 = CARTESIAN_POINT ( 'NONE',  ( 10.18405858231679595, -20.26807450282662160, 1.696391591240633101 ) ) ;
#8246 = CARTESIAN_POINT ( 'NONE',  ( 12.62599079447150885, -20.19996487918709249, 4.820256282269618886 ) ) ;
#8247 = CARTESIAN_POINT ( 'NONE',  ( -13.15498530132288479, 5.764257716805535559, 2.999999999999999556 ) ) ;
#8248 = EDGE_LOOP ( 'NONE', ( #12616, #9706, #5886, #8941 ) ) ;
#8249 = VECTOR ( 'NONE', #13209, 1000.000000000000000 ) ;
#8250 = PLANE ( 'NONE',  #13281 ) ;
#8251 = ADVANCED_FACE ( 'NONE', ( #3189 ), #14681, .T. ) ;
#8252 = LINE ( 'NONE', #11277, #10997 ) ;
#8253 = EDGE_CURVE ( 'NONE', #18307, #12822, #3284, .T. ) ;
#8254 = ORIENTED_EDGE ( 'NONE', *, *, #15314, .F. ) ;
#8255 = AXIS2_PLACEMENT_3D ( 'NONE', #5920, #9066, #900 ) ;
#8256 = VERTEX_POINT ( 'NONE', #19409 ) ;
#8257 = CARTESIAN_POINT ( 'NONE',  ( 2.601332995093193379, -9.970398767539743190, 2.592349323443654097 ) ) ;
#8258 = ORIENTED_EDGE ( 'NONE', *, *, #18205, .F. ) ;
#8259 = CARTESIAN_POINT ( 'NONE',  ( -5.965308582316793284, -20.22900456129164937, 4.174186261275266929 ) ) ;
#8260 = CARTESIAN_POINT ( 'NONE',  ( 13.11017182064853159, 4.251176942750957366, 5.979809059808775196 ) ) ;
#8261 = CARTESIAN_POINT ( 'NONE',  ( -9.000000000000000000, -9.999999999999992895, 2.000000000000000000 ) ) ;
#8262 = CARTESIAN_POINT ( 'NONE',  ( 12.62499999999998224, -20.24999999999998934, 4.291666666666698937 ) ) ;
#8263 = CARTESIAN_POINT ( 'NONE',  ( -7.369520639128046113, 4.999999999999999112, 1.000000000000000000 ) ) ;
#8264 = CARTESIAN_POINT ( 'NONE',  ( -13.81612658856640863, 2.776892722604777930, 5.216624963382545666 ) ) ;
#8265 = CARTESIAN_POINT ( 'NONE',  ( 7.652808582316796837, -20.91377862118960351, 5.979004561291660913 ) ) ;
#8266 = CARTESIAN_POINT ( 'NONE',  ( -13.15498530132288479, 5.764257716805535559, 4.583333333333295734 ) ) ;
#8267 = CARTESIAN_POINT ( 'NONE',  ( -7.652808582316796837, -20.91377862118960351, 5.979004561291660913 ) ) ;
#8268 = CARTESIAN_POINT ( 'NONE',  ( -15.49999999999999822, -22.99999999999999289, 4.000000000000000000 ) ) ;
#8269 = CARTESIAN_POINT ( 'NONE',  ( 0.000000000000000000, 16.00000000000000000, 1.000000000000000000 ) ) ;
#8270 = CARTESIAN_POINT ( 'NONE',  ( 7.184058582316795949, -21.32873467460644079, 2.757051763020455404 ) ) ;
#8271 = CARTESIAN_POINT ( 'NONE',  ( -9.534691417683177406, -20.22900456129164581, 2.825813738724748170 ) ) ;
#8272 = EDGE_LOOP ( 'NONE', ( #1384, #4803, #3160, #20126 ) ) ;
#8273 = ADVANCED_FACE ( 'NONE', ( #6538 ), #1923, .T. ) ;
#8274 = ORIENTED_EDGE ( 'NONE', *, *, #4716, .T. ) ;
#8275 = CARTESIAN_POINT ( 'NONE',  ( 13.37499999999998579, -20.24999999999999289, 3.666666666666653640 ) ) ;
#8276 = CARTESIAN_POINT ( 'NONE',  ( -9.305650798910056309, 4.999999999999999112, 0.000000000000000000 ) ) ;
#8277 = ORIENTED_EDGE ( 'NONE', *, *, #10161, .T. ) ;
#8278 = EDGE_LOOP ( 'NONE', ( #15513, #15453, #11355, #4535 ) ) ;
#8279 = CARTESIAN_POINT ( 'NONE',  ( 1.937849085826861328, 16.00000000000000000, 1.000000000000000000 ) ) ;
#8280 = LINE ( 'NONE', #16233, #5351 ) ;
#8281 = VECTOR ( 'NONE', #12306, 1000.000000000000000 ) ;
#8282 = CARTESIAN_POINT ( 'NONE',  ( -13.12529397354238192, 5.014845663890297622, 3.999999999999981792 ) ) ;
#8283 = DIRECTION ( 'NONE',  ( 0.000000000000000000, -1.000000000000000000, 0.000000000000000000 ) ) ;
#8284 = EDGE_CURVE ( 'NONE', #13535, #15823, #20663, .T. ) ;
#8285 = CARTESIAN_POINT ( 'NONE',  ( -23.35856191738413656, 4.999999999999999112, 1.000000000000000000 ) ) ;
#8286 = CARTESIAN_POINT ( 'NONE',  ( -13.02818618459764188, 0.1109023222084986743, 5.923858176248589125 ) ) ;
#8287 = CARTESIAN_POINT ( 'NONE',  ( 6.809058582316794173, -23.27327832286945153, 2.298404588716537411 ) ) ;
#8288 = DIRECTION ( 'NONE',  ( 0.000000000000000000, -0.000000000000000000, 1.000000000000000000 ) ) ;
#8289 = CARTESIAN_POINT ( 'NONE',  ( 13.08094078691552831, 2.775009739235173356, 5.981149842915306714 ) ) ;
#8290 = STYLED_ITEM ( 'NONE', ( #11480 ), #17970 ) ;
#8291 = CARTESIAN_POINT ( 'NONE',  ( -1.126276606324276619, -9.864917468222230923, 2.372643865078341019 ) ) ;
#8292 = ORIENTED_EDGE ( 'NONE', *, *, #11710, .T. ) ;
#8293 = CARTESIAN_POINT ( 'NONE',  ( -13.84504075139246915, 3.487057945321567765, 5.981929699623240282 ) ) ;
#8294 = PLANE ( 'NONE',  #7393 ) ;
#8295 = CARTESIAN_POINT ( 'NONE',  ( 8.409691417683177406, -21.32581373872474373, 5.270995438708348857 ) ) ;
#8296 = CARTESIAN_POINT ( 'NONE',  ( -9.246558582316795949, -21.94931252712234127, 4.499999999999999112 ) ) ;
#8297 = ORIENTED_EDGE ( 'NONE', *, *, #15091, .F. ) ;
#8298 = CARTESIAN_POINT ( 'NONE',  ( 13.56222317325195093, -11.54522975075300728, 6.408692769197242178 ) ) ;
#8299 = CARTESIAN_POINT ( 'NONE',  ( 13.11145189917479392, 4.315820908324673688, 5.961432613039677086 ) ) ;
#8300 = CARTESIAN_POINT ( 'NONE',  ( -13.87470602645761808, 4.985154336109792972, 4.000000000000000000 ) ) ;
#8301 = ORIENTED_EDGE ( 'NONE', *, *, #2501, .F. ) ;
#8302 = ORIENTED_EDGE ( 'NONE', *, *, #13952, .T. ) ;
#8303 = DIRECTION ( 'NONE',  ( -0.000000000000000000, -0.000000000000000000, -1.000000000000000000 ) ) ;
#8304 = VECTOR ( 'NONE', #80, 1000.000000000000000 ) ;
#8305 = DIRECTION ( 'NONE',  ( -1.000000000000000000, -8.673617379884045333E-17, 0.000000000000000000 ) ) ;
#8306 = AXIS2_PLACEMENT_3D ( 'NONE', #13017, #6447, #11243 ) ;
#8307 = CARTESIAN_POINT ( 'NONE',  ( 0.6250000000000005551, 10.00000000000000000, 1.000000000000000000 ) ) ;
#8308 = LINE ( 'NONE', #5265, #1319 ) ;
#8309 = CARTESIAN_POINT ( 'NONE',  ( 2.088806020750596737, -10.42712783963456857, 1.767030719737609168 ) ) ;
#8310 = CARTESIAN_POINT ( 'NONE',  ( 0.000000000000000000, 10.00000000000000000, 1.000000000000000000 ) ) ;
#8311 = DIRECTION ( 'NONE',  ( -6.938893903907222067E-15, 1.000000000000000000, 0.000000000000000000 ) ) ;
#8312 = ADVANCED_FACE ( 'NONE', ( #6745 ), #51, .T. ) ;
#8313 = DIRECTION ( 'NONE',  ( 1.000000000000000000, 0.000000000000000000, 0.000000000000000000 ) ) ;
#8314 = LINE ( 'NONE', #17622, #3302 ) ;
#8315 = FACE_OUTER_BOUND ( 'NONE', #15265, .T. ) ;
#8316 = CARTESIAN_POINT ( 'NONE',  ( -3.187906586576829682, -9.105473976199601083, 1.812833570429532859 ) ) ;
#8317 = VECTOR ( 'NONE', #18032, 1000.000000000000000 ) ;
#8318 = ORIENTED_EDGE ( 'NONE', *, *, #19045, .F. ) ;
#8319 = CARTESIAN_POINT ( 'NONE',  ( -12.62691554569741648, -19.40326494227377907, 4.703927990036796736 ) ) ;
#8320 = CARTESIAN_POINT ( 'NONE',  ( -10.65280858231679240, -21.22443879296942626, 5.229004561291659137 ) ) ;
#8321 = CARTESIAN_POINT ( 'NONE',  ( -8.503441417683177406, -22.05068747287765873, 5.250000000000000888 ) ) ;
#8322 = AXIS2_PLACEMENT_3D ( 'NONE', #16731, #10565, #16933 ) ;
#8323 = ORIENTED_EDGE ( 'NONE', *, *, #11576, .T. ) ;
#8324 = CARTESIAN_POINT ( 'NONE',  ( 13.84501469867711698, 4.235742283194553259, 4.666666666666618113 ) ) ;
#8325 = CARTESIAN_POINT ( 'NONE',  ( 7.499999999999999112, -25.49999999999999645, 6.500000000000000888 ) ) ;
#8326 = ORIENTED_EDGE ( 'NONE', *, *, #13695, .T. ) ;
#8327 = ORIENTED_EDGE ( 'NONE', *, *, #19609, .F. ) ;
#8328 = CARTESIAN_POINT ( 'NONE',  ( 27.44203811574919882, 10.00000000000000000, 1.000000000000000000 ) ) ;
#8329 = ORIENTED_EDGE ( 'NONE', *, *, #6971, .F. ) ;
#8330 = CARTESIAN_POINT ( 'NONE',  ( -5.000000000000000000, 0.000000000000000000, 0.000000000000000000 ) ) ;
#8331 = VECTOR ( 'NONE', #9365, 1000.000000000000000 ) ;
#8332 = VERTEX_POINT ( 'NONE', #4958 ) ;
#8333 = CARTESIAN_POINT ( 'NONE',  ( 5.503441417683176518, -22.05068747287765873, 5.250000000000000888 ) ) ;
#8334 = CARTESIAN_POINT ( 'NONE',  ( -5.381197846483055436, -6.000000000000000000, 2.000000000000000000 ) ) ;
#8335 = AXIS2_PLACEMENT_3D ( 'NONE', #17581, #3256, #12974 ) ;
#8336 = CARTESIAN_POINT ( 'NONE',  ( -1.126276606324276619, -9.864917468222230923, 2.372643865078341019 ) ) ;
#8337 = LINE ( 'NONE', #12831, #7336 ) ;
#8338 = CARTESIAN_POINT ( 'NONE',  ( -7.559058582316794173, -20.72672167713054137, 4.701595411283463477 ) ) ;
#8339 = VECTOR ( 'NONE', #12513, 1000.000000000000000 ) ;
#8340 = EDGE_CURVE ( 'NONE', #2700, #12487, #11338, .T. ) ;
#8341 = CARTESIAN_POINT ( 'NONE',  ( 3.747260319564023501, 0.000000000000000000, 1.000000000000000000 ) ) ;
#8342 = CARTESIAN_POINT ( 'NONE',  ( 10.28469141768318096, -23.77099543870834353, 4.174186261275252718 ) ) ;
#8343 = LINE ( 'NONE', #13149, #14216 ) ;
#8344 = CARTESIAN_POINT ( 'NONE',  ( -4.003441417683176518, -22.05068747287765873, 5.250000000000000888 ) ) ;
#8345 = ORIENTED_EDGE ( 'NONE', *, *, #14717, .T. ) ;
#8346 = CARTESIAN_POINT ( 'NONE',  ( 8.965308582316795949, -19.47900456129164937, 4.484846433055089676 ) ) ;
#8347 = EDGE_CURVE ( 'NONE', #7660, #19894, #247, .T. ) ;
#8348 = CARTESIAN_POINT ( 'NONE',  ( 13.08573665985359824, 3.017201322601628100, 5.986358176248492313 ) ) ;
#8349 = CARTESIAN_POINT ( 'NONE',  ( -13.15498501280115917, 5.764243146453090105, 5.045733045595949484 ) ) ;
#8350 = VECTOR ( 'NONE', #14062, 1000.000000000000114 ) ;
#8351 = VERTEX_POINT ( 'NONE', #10394 ) ;
#8352 = EDGE_CURVE ( 'NONE', #12771, #20538, #9970, .T. ) ;
#8353 = CARTESIAN_POINT ( 'NONE',  ( 19.23630159782011617, 4.999999999999999112, 1.000000000000000000 ) ) ;
#8354 = DIRECTION ( 'NONE',  ( 0.000000000000000000, 0.000000000000000000, 1.000000000000000000 ) ) ;
#8355 = MECHANICAL_DESIGN_GEOMETRIC_PRESENTATION_REPRESENTATION (  '', ( #7696 ), #11363 ) ;
#8356 = VERTEX_POINT ( 'NONE', #6839 ) ;
#8357 = APPLICATION_PROTOCOL_DEFINITION ( 'draft international standard', 'automotive_design', 1998, #12272 ) ;
#8358 = VERTEX_POINT ( 'NONE', #4009 ) ;
#8359 = AXIS2_PLACEMENT_3D ( 'NONE', #6180, #4601, #19259 ) ;
#8360 = CARTESIAN_POINT ( 'NONE',  ( 13.26926852418574754, -19.98898271615830424, 3.463267919252106974 ) ) ;
#8361 = ORIENTED_EDGE ( 'NONE', *, *, #4002, .F. ) ;
#8362 = LINE ( 'NONE', #5321, #12640 ) ;
#8363 = CARTESIAN_POINT ( 'NONE',  ( -12.50209451496117197, 10.00000000000000000, 0.000000000000000000 ) ) ;
#8364 = VECTOR ( 'NONE', #13931, 1000.000000000000000 ) ;
#8365 = PLANE ( 'NONE',  #15465 ) ;
#8366 = EDGE_CURVE ( 'NONE', #19354, #10019, #17923, .T. ) ;
#8367 = CARTESIAN_POINT ( 'NONE',  ( 13.15492785973632017, 5.761356916681801721, 5.116543252045025802 ) ) ;
#8368 = LINE ( 'NONE', #19158, #452 ) ;
#8369 = CARTESIAN_POINT ( 'NONE',  ( 0.000000000000000000, 11.64110105645932691, 10.00000000000000000 ) ) ;
#8370 = CARTESIAN_POINT ( 'NONE',  ( -13.37500015856764435, -20.24999199233421265, 4.532157119432948633 ) ) ;
#8371 = VECTOR ( 'NONE', #18537, 1000.000000000000000 ) ;
#8372 = CARTESIAN_POINT ( 'NONE',  ( 9.809058582316795949, -23.80360840875935935, 1.768074502826626260 ) ) ;
#8373 = CARTESIAN_POINT ( 'NONE',  ( -13.09546733092777160, 2.758600211853326822, 6.730829579156167419 ) ) ;
#8374 = CARTESIAN_POINT ( 'NONE',  ( -7.090308582316795061, -21.01515356694490322, 0.9790045612916562501 ) ) ;
#8375 = VECTOR ( 'NONE', #19994, 1000.000000000000000 ) ;
#8376 = LINE ( 'NONE', #13173, #3043 ) ;
#8377 = PLANE ( 'NONE',  #5411 ) ;
#8378 = CARTESIAN_POINT ( 'NONE',  ( 9.246558582316795949, -21.94931252712234127, 4.499999999999999112 ) ) ;
#8379 = CARTESIAN_POINT ( 'NONE',  ( -4.847191417683178294, -21.22443879296941915, 1.770995438708345748 ) ) ;
#8380 = ORIENTED_EDGE ( 'NONE', *, *, #10196, .F. ) ;
#8381 = ORIENTED_EDGE ( 'NONE', *, *, #15654, .F. ) ;
#8382 = CARTESIAN_POINT ( 'NONE',  ( 13.38921792038197900, -19.53199502070850357, 5.456033026503027017 ) ) ;
#8383 = CARTESIAN_POINT ( 'NONE',  ( 13.50000000000001243, -24.49999999999999289, 4.000000000000000000 ) ) ;
#8384 = CARTESIAN_POINT ( 'NONE',  ( -7.369520639128046113, 9.000000000000001776, 1.000000000000000000 ) ) ;
#8385 = ORIENTED_EDGE ( 'NONE', *, *, #11684, .F. ) ;
#8386 = ADVANCED_FACE ( 'NONE', ( #7156 ), #13520, .T. ) ;
#8387 = DIRECTION ( 'NONE',  ( -0.000000000000000000, -0.000000000000000000, -1.000000000000000000 ) ) ;
#8388 = PLANE ( 'NONE',  #1681 ) ;
#8389 = VECTOR ( 'NONE', #12690, 1000.000000000000000 ) ;
#8390 = AXIS2_PLACEMENT_3D ( 'NONE', #4945, #11027, #3078 ) ;
#8391 = CARTESIAN_POINT ( 'NONE',  ( 13.84504075139246915, 3.487057945321567765, 5.981929699623240282 ) ) ;
#8392 = B_SPLINE_CURVE_WITH_KNOTS ( 'NONE', 3,
 ( #12367, #17271, #13723, #7465, #12159, #17177, #4318, #4523, #1084, #18548, #7774, #12060, #10703, #4425, #2854, #10909, #2754, #18450, #2952, #14137, #5991, #20444, #20542, #10811, #4113, #10496, #16965, #16864, #9229, #1183, #9332, #17074, #13824, #15401, #7361, #15709, #14034, #5789, #2533, #8923, #18762, #15292, #20227, #6100, #4213, #10593, #1285, #2642, #7562, #5888, #12258, #18651, #15600, #12468, #18863, #9132, #15502, #13926, #20328, #8084, #17588, #1588, #5042, #17383, #14552, #17696, #4727, #3370, #7965, #16234, #19381, #11420, #17804, #12666, #3470, #224, #9637, #17485, #16131, #3166, #9848, #8282 ),
 .UNSPECIFIED., .F., .F.,
 ( 4, 2, 2, 2, 2, 2, 2, 2, 2, 2, 2, 2, 2, 2, 2, 2, 2, 2, 2, 2, 2, 2, 2, 2, 2, 2, 2, 2, 2, 2, 2, 2, 2, 2, 2, 2, 2, 2, 2, 2, 4 ),
 ( 0.03648247254878290990, 0.05122453910963482848, 0.05943139484297973313, 0.06353482270965218892, 0.06763825057632463778, 0.07081696859385248899, 0.07399568661138034020, 0.08035312264643605651, 0.09306799471654747524, 0.1057828667866588801, 0.1121403028217145964, 0.1153190208392424337, 0.1184977388567702850, 0.1214804596100246964, 0.1244631803632790940, 0.1304286218697879030, 0.1423595048828055210, 0.1662212709088407014, 0.2139448029609111179, 0.3093918670650518954, 0.5002859952733336169, 0.6911801234816151718, 0.7866271875857560048, 0.8343507196378263657, 0.8582124856638615462, 0.8701433686768791365, 0.8761088101833880426, 0.8790915309366424957, 0.8820742516898969487, 0.8853411830926060100, 0.8886081144953148492, 0.8951419773007329717, 0.9082097029115692166, 0.9212774285224054616, 0.9278112913278236951, 0.9310782227305326453, 0.9343451541332417065, 0.9384485819999140999, 0.9425520098665866042, 0.9507588655999313909, 0.9671725770666211863 ),
 .UNSPECIFIED. ) ;
#8393 = AXIS2_PLACEMENT_3D ( 'NONE', #4196, #15275, #4408 ) ;
#8394 = LINE ( 'NONE', #7694, #14526 ) ;
#8395 = CARTESIAN_POINT ( 'NONE',  ( 3.951988298270009636, -13.15210598010094323, 2.852089508627633219 ) ) ;
#8396 = AXIS2_PLACEMENT_3D ( 'NONE', #10088, #17832, #775 ) ;
#8397 = EDGE_CURVE ( 'NONE', #20714, #14757, #2560, .T. ) ;
#8398 = EDGE_CURVE ( 'NONE', #8135, #5810, #3591, .T. ) ;
#8399 = CARTESIAN_POINT ( 'NONE',  ( 1.619022621591187150, -9.114917468222230923, 1.622643865078341463 ) ) ;
#8400 = CARTESIAN_POINT ( 'NONE',  ( -12.64387510712649565, -19.29680709011273976, 5.506486987317513737 ) ) ;
#8401 = CARTESIAN_POINT ( 'NONE',  ( 9.434058582316794173, -23.20159541128345992, 4.773278322869455970 ) ) ;
#8402 = CARTESIAN_POINT ( 'NONE',  ( 19.73630159782011617, 4.999999999999999112, 1.000000000000000000 ) ) ;
#8403 = CARTESIAN_POINT ( 'NONE',  ( 13.11740841389447709, 4.616624901677048420, 5.813473370769506765 ) ) ;
#8404 = ADVANCED_FACE ( 'NONE', ( #16764 ), #8613, .F. ) ;
#8405 = CARTESIAN_POINT ( 'NONE',  ( -1.717920576997000737, -9.114924032904250240, 2.372645551019823884 ) ) ;
#8406 = LINE ( 'NONE', #3579, #10060 ) ;
#8407 = CIRCLE ( 'NONE', #16740, 10.00000000000000000 ) ;
#8408 = CARTESIAN_POINT ( 'NONE',  ( 7.472191417683176518, -23.72900456129165292, 2.724438792969417822 ) ) ;
#8409 = CARTESIAN_POINT ( 'NONE',  ( -8.496558582316795949, -22.05068747287764452, 2.499999999999999112 ) ) ;
#8410 = EDGE_LOOP ( 'NONE', ( #7275, #15493, #13821, #7071 ) ) ;
#8411 = CARTESIAN_POINT ( 'NONE',  ( 13.79242507427300879, 0.07996625081441015304, 6.658692769197546824 ) ) ;
#8412 = CARTESIAN_POINT ( 'NONE',  ( 13.08094078691552831, 2.775009739235173356, 5.981149842915306714 ) ) ;
#8413 = LINE ( 'NONE', #5160, #16351 ) ;
#8414 = ORIENTED_EDGE ( 'NONE', *, *, #301, .T. ) ;
#8415 = ADVANCED_FACE ( 'NONE', ( #19922 ), #5685, .T. ) ;
#8416 = ORIENTED_EDGE ( 'NONE', *, *, #5009, .F. ) ;
#8417 = CARTESIAN_POINT ( 'NONE',  ( 13.49999999999998401, -18.49999999999999645, 4.000000000000000000 ) ) ;
#8418 = CARTESIAN_POINT ( 'NONE',  ( 3.499999999999998668, -19.50000000000000000, 1.000000000000000000 ) ) ;
#8419 = CARTESIAN_POINT ( 'NONE',  ( 21.67243175760212637, 0.000000000000000000, 1.000000000000000000 ) ) ;
#8420 = VECTOR ( 'NONE', #4178, 1000.000000000000000 ) ;
#8421 = CARTESIAN_POINT ( 'NONE',  ( 0.000000000000000000, 11.64110105645932691, 10.00000000000000000 ) ) ;
#8422 = CARTESIAN_POINT ( 'NONE',  ( 2.167793999318431197, -10.98794063836983703, 1.911058649813994315 ) ) ;
#8423 = CARTESIAN_POINT ( 'NONE',  ( 0.000000000000000000, 9.000000000000001776, 1.000000000000000000 ) ) ;
#8424 = LINE ( 'NONE', #13317, #20105 ) ;
#8425 =( BOUNDED_SURFACE ( )  B_SPLINE_SURFACE ( 3, 3, ( 
 ( #15619, #1302, #10722, #20658, #11133, #6315, #9152, #17502, #14053, #9458, #2772, #12489, #17404, #12277, #10927, #17095, #15929, #1411, #14155, #15520, #7792, #3084, #15830, #1507, #14248, #1606, #19403, #19602, #11538, #6834, #14569, #13203, #2022, #5061, #14779, #6430, #353, #12894, #9658, #16153, #14359, #1720, #16347, #16045, #242, #17607, #13105, #4951, #6740, #8412, #6631, #17822, #11632, #7987, #13000, #3389, #14468, #456, #1817, #147, #3279, #16249, #3489, #45, #8299, #6533, #19508, #8104, #11438, #19298, #9865, #1918, #14673, #8203, #5255, #12794, #11330, #17718, #5159, #19196, #18022, #9767, #3584, #17917, #9965, #3693 ),
 ( #10077, #16451, #4849, #11230, #2429, #7352, #3799, #18233, #2222, #7248, #4001, #10275, #654, #5678, #12152, #2125, #15083, #15188, #13610, #15285, #13514, #19701, #19916, #4106, #7043, #19816, #8821, #6933, #8506, #12050, #16546, #18134, #13714, #11842, #13411, #16644, #18337, #14877, #10588, #5470, #3896, #18543, #865, #18445, #8606, #2323, #8917, #10176, #5570, #11941, #10386, #20014, #10489, #8712, #16758, #16859, #765, #20121, #2526, #5783, #4206, #963, #554, #13300, #5364, #14977, #11742, #7151, #4419, #4310, #5984, #17172, #1277, #6095, #4720, #20221, #20321, #5882, #12557, #10903, #2945, #16956, #20436, #9126, #10695, #4611 ),
 ( #12252, #9433, #2635, #15495, #14131, #2848, #9223, #18644, #7657, #15593, #2746, #11004, #12359, #10803, #6287, #18857, #7862, #17373, #18956, #17265, #12659, #4518, #15806, #17066, #9022, #20632, #3059, #7766, #1178, #15393, #20536, #12463, #1483, #14027, #18753, #13919, #7458, #9325, #15701, #1385, #1078, #13819, #6189, #14224, #19062, #7556, #11410, #19578, #123, #3562, #14, #218, #9530, #12972, #17689, #11109, #14754, #6402, #15902, #17480, #17895, #1581, #3462, #16013, #12769, #19272, #3158, #4826, #19482, #19172, #3360, #11207, #16227, #8076, #9840, #11514, #9740, #6604, #432, #7957, #16124, #6508, #17580, #9942, #4924, #3254 ),
 ( #14546, #1894, #6811, #8275, #9628, #19375, #16323, #11303, #1691, #12870, #1791, #8178, #5030, #14330, #14441, #17796, #14646, #6711, #326, #13080, #5136, #1997, #8382, #13180, #13587, #3974, #2101, #11817, #529, #18420, #11610, #3774, #2407, #18210, #3872, #8484, #16618, #5448, #11715, #19988, #631, #19790, #15263, #7128, #16837, #5652, #841, #5547, #941, #13490, #4082, #19676, #17996, #8897, #7224, #16734, #10153, #3667, #8798, #15060, #10470, #10250, #7019, #2198, #16424, #2298, #8689, #8581, #10051, #14853, #11917, #742, #19891, #2503, #18308, #13689, #14950, #7328, #6907, #10360, #13275, #15166, #12024, #5232, #5340, #18111 ),
 ( #16524, #13386, #5863, #18624, #2827, #18524, #20098, #6072, #7436, #9103, #12232, #20410, #75, #5761, #13900, #7632, #14005, #9303, #12334, #12132, #2722, #4184, #15475, #4397, #20300, #1258, #16936, #5960, #18730, #6461, #1640, #4284, #17150, #7534, #10569, #15370, #15679, #1157, #10780, #13798, #2608, #8999, #1054, #9200, #20202, #12440, #10671, #15574, #18834, #17044, #17245, #4497, #2925, #10882, #8021, #14391, #3735, #7188, #16799, #10430, #11780, #5723, #19952, #8757, #8953, #901, #16897, #3934, #2568, #12093, #15130, #4145, #16489, #2468, #2259, #19748, #5505, #10115, #18170, #18484, #5406, #10320, #6977, #8859, #15020, #15227 ),
 ( #1008, #18069, #2369, #13451, #3835, #10528, #11880, #10214, #13347, #5610, #13551, #2161, #18384, #16582, #7286, #8646, #804, #700, #11984, #4046, #13648, #18272, #15327, #8545, #7086, #19855, #16690, #14915, #7399, #20060, #13760, #20163, #5824, #592, #3173, #17493, #3072, #3377, #232, #7878, #7975, #12784, #17705, #14145, #14237, #12572, #17597, #14348, #1595, #12191, #15716, #15819, #1399, #8092, #6420, #19186, #18583, #15918, #4627, #6203, #138, #11221, #9340, #19079, #7782, #4941, #4532, #11021, #9646, #4735, #11123, #20552, #9547, #12676, #18972, #6522, #20645, #6303, #1808, #32, #9756, #12885, #14458, #4840, #8193, #3270 ),
 ( #10916, #16032, #1708, #16141, #19288, #17390, #11321, #14559, #17279, #2963, #9448, #1497, #14770, #17812, #13402, #3887, #19808, #1906, #11835, #2014, #2214, #16240, #13195, #19693, #5050, #11624, #19392, #8704, #19593, #6923, #12991, #16442, #5356, #11734, #344, #14966, #8499, #18014, #18225, #10169, #5463, #5247, #10267, #647, #3685, #16634, #11427, #18126, #11528, #8289, #447, #3478, #6728, #7035, #14664, #10069, #13095, #3792, #3576, #16539, #2314, #2117, #14869, #15075, #6620, #544, #8403, #19498, #9855, #6826, #5150, #17909, #13292, #8596, #9955, #16340, #15331, #2571, #1011, #17112, #7704, #2683, #8956, #4249, #15441, #20265 ) ),
 .UNSPECIFIED., .T., .F., .T. ) 
 B_SPLINE_SURFACE_WITH_KNOTS ( ( 4, 3, 4 ),
 ( 4, 2, 2, 2, 2, 2, 2, 2, 2, 2, 2, 2, 2, 2, 2, 2, 2, 2, 2, 2, 2, 2, 2, 2, 2, 2, 2, 2, 2, 2, 2, 2, 2, 2, 2, 2, 2, 2, 2, 2, 2, 2, 4 ),
 ( 0.000000000000000000, 0.5000000000000000000, 1.000000000000000000 ),
 ( 0.000000000000000000, 0.03481082764294501225, 0.05122453910963481460, 0.05943139484297971231, 0.06353482270965216117, 0.06763825057632461002, 0.07081696859385246123, 0.07399568661138031245, 0.08035312264643601488, 0.09306799471654741973, 0.1057828667866588246, 0.1121403028217145270, 0.1153190208392423644, 0.1184977388567702156, 0.1214804596100246270, 0.1244631803632790246, 0.1304286218697878197, 0.1423595048828054099, 0.1662212709088405904, 0.2139448029609109514, 0.3093918670650516733, 0.5002859952733331728, 0.6911801234816146167, 0.7866271875857553386, 0.8343507196378256996, 0.8582124856638608801, 0.8701433686768784703, 0.8761088101833873765, 0.8790915309366418295, 0.8820742516898961716, 0.8853411830926052328, 0.8886081144953141830, 0.8951419773007323055, 0.9082097029115685505, 0.9212774285224047954, 0.9278112913278229179, 0.9310782227305318681, 0.9343451541332409294, 0.9384485819999133227, 0.9425520098665858271, 0.9507588655999306138, 0.9671725770666204092, 1.000000000000000000 ),
 .UNSPECIFIED. ) 
 GEOMETRIC_REPRESENTATION_ITEM ( )  RATIONAL_B_SPLINE_SURFACE ( (
 ( 1.000000000000000000, 1.000000000000000000, 1.000000000000000000, 1.000000000000000000, 1.000000000000000000, 1.000000000000000000, 1.000000000000000000, 1.000000000000000000, 1.000000000000000000, 1.000000000000000000, 1.000000000000000000, 1.000000000000000000, 1.000000000000000000, 1.000000000000000000, 1.000000000000000000, 1.000000000000000000, 1.000000000000000000, 1.000000000000000000, 1.000000000000000000, 1.000000000000000000, 1.000000000000000000, 1.000000000000000000, 1.000000000000000000, 1.000000000000000000, 1.000000000000000000, 1.000000000000000000, 1.000000000000000000, 1.000000000000000000, 1.000000000000000000, 1.000000000000000000, 1.000000000000000000, 1.000000000000000000, 1.000000000000000000, 1.000000000000000000, 1.000000000000000000, 1.000000000000000000, 1.000000000000000000, 1.000000000000000000, 1.000000000000000000, 1.000000000000000000, 1.000000000000000000, 1.000000000000000000, 1.000000000000000000, 1.000000000000000000, 1.000000000000000000, 1.000000000000000000, 1.000000000000000000, 1.000000000000000000, 1.000000000000000000, 1.000000000000000000, 1.000000000000000000, 1.000000000000000000, 1.000000000000000000, 1.000000000000000000, 1.000000000000000000, 1.000000000000000000, 1.000000000000000000, 1.000000000000000000, 1.000000000000000000, 1.000000000000000000, 1.000000000000000000, 1.000000000000000000, 1.000000000000000000, 1.000000000000000000, 1.000000000000000000, 1.000000000000000000, 1.000000000000000000, 1.000000000000000000, 1.000000000000000000, 1.000000000000000000, 1.000000000000000000, 1.000000000000000000, 1.000000000000000000, 1.000000000000000000, 1.000000000000000000, 1.000000000000000000, 1.000000000000000000, 1.000000000000000000, 1.000000000000000000, 1.000000000000000000, 1.000000000000000000, 1.000000000000000000, 1.000000000000000000, 1.000000000000000000, 1.000000000000000000, 1.000000000000000000),
 ( 0.3333333333333333703, 0.3333333333333333703, 0.3333333333333333703, 0.3333333333333333703, 0.3333333333333333703, 0.3333333333333333703, 0.3333333333333333703, 0.3333333333333333703, 0.3333333333333333703, 0.3333333333333333703, 0.3333333333333333703, 0.3333333333333333703, 0.3333333333333333703, 0.3333333333333333703, 0.3333333333333333703, 0.3333333333333333703, 0.3333333333333333703, 0.3333333333333333703, 0.3333333333333333703, 0.3333333333333333703, 0.3333333333333333703, 0.3333333333333333703, 0.3333333333333333703, 0.3333333333333333703, 0.3333333333333333703, 0.3333333333333333703, 0.3333333333333333703, 0.3333333333333333703, 0.3333333333333333703, 0.3333333333333333703, 0.3333333333333333703, 0.3333333333333333703, 0.3333333333333333703, 0.3333333333333333703, 0.3333333333333333703, 0.3333333333333333703, 0.3333333333333333703, 0.3333333333333333703, 0.3333333333333333703, 0.3333333333333333703, 0.3333333333333333703, 0.3333333333333333703, 0.3333333333333333703, 0.3333333333333333703, 0.3333333333333333703, 0.3333333333333333703, 0.3333333333333333703, 0.3333333333333333703, 0.3333333333333333703, 0.3333333333333333703, 0.3333333333333333703, 0.3333333333333333703, 0.3333333333333333703, 0.3333333333333333703, 0.3333333333333333703, 0.3333333333333333703, 0.3333333333333333703, 0.3333333333333333703, 0.3333333333333333703, 0.3333333333333333703, 0.3333333333333333703, 0.3333333333333333703, 0.3333333333333333703, 0.3333333333333333703, 0.3333333333333333703, 0.3333333333333333703, 0.3333333333333333703, 0.3333333333333333703, 0.3333333333333333703, 0.3333333333333333703, 0.3333333333333333703, 0.3333333333333333703, 0.3333333333333333703, 0.3333333333333333703, 0.3333333333333333703, 0.3333333333333333703, 0.3333333333333333703, 0.3333333333333333703, 0.3333333333333333703, 0.3333333333333333703, 0.3333333333333333703, 0.3333333333333333703, 0.3333333333333333703, 0.3333333333333333703, 0.3333333333333333703, 0.3333333333333333703),
 ( 0.3333333333333333703, 0.3333333333333333703, 0.3333333333333333703, 0.3333333333333333703, 0.3333333333333333703, 0.3333333333333333703, 0.3333333333333333703, 0.3333333333333333703, 0.3333333333333333703, 0.3333333333333333703, 0.3333333333333333703, 0.3333333333333333703, 0.3333333333333333703, 0.3333333333333333703, 0.3333333333333333703, 0.3333333333333333703, 0.3333333333333333703, 0.3333333333333333703, 0.3333333333333333703, 0.3333333333333333703, 0.3333333333333333703, 0.3333333333333333703, 0.3333333333333333703, 0.3333333333333333703, 0.3333333333333333703, 0.3333333333333333703, 0.3333333333333333703, 0.3333333333333333703, 0.3333333333333333703, 0.3333333333333333703, 0.3333333333333333703, 0.3333333333333333703, 0.3333333333333333703, 0.3333333333333333703, 0.3333333333333333703, 0.3333333333333333703, 0.3333333333333333703, 0.3333333333333333703, 0.3333333333333333703, 0.3333333333333333703, 0.3333333333333333703, 0.3333333333333333703, 0.3333333333333333703, 0.3333333333333333703, 0.3333333333333333703, 0.3333333333333333703, 0.3333333333333333703, 0.3333333333333333703, 0.3333333333333333703, 0.3333333333333333703, 0.3333333333333333703, 0.3333333333333333703, 0.3333333333333333703, 0.3333333333333333703, 0.3333333333333333703, 0.3333333333333333703, 0.3333333333333333703, 0.3333333333333333703, 0.3333333333333333703, 0.3333333333333333703, 0.3333333333333333703, 0.3333333333333333703, 0.3333333333333333703, 0.3333333333333333703, 0.3333333333333333703, 0.3333333333333333703, 0.3333333333333333703, 0.3333333333333333703, 0.3333333333333333703, 0.3333333333333333703, 0.3333333333333333703, 0.3333333333333333703, 0.3333333333333333703, 0.3333333333333333703, 0.3333333333333333703, 0.3333333333333333703, 0.3333333333333333703, 0.3333333333333333703, 0.3333333333333333703, 0.3333333333333333703, 0.3333333333333333703, 0.3333333333333333703, 0.3333333333333333703, 0.3333333333333333703, 0.3333333333333333703, 0.3333333333333333703),
 ( 1.000000000000000000, 1.000000000000000000, 1.000000000000000000, 1.000000000000000000, 1.000000000000000000, 1.000000000000000000, 1.000000000000000000, 1.000000000000000000, 1.000000000000000000, 1.000000000000000000, 1.000000000000000000, 1.000000000000000000, 1.000000000000000000, 1.000000000000000000, 1.000000000000000000, 1.000000000000000000, 1.000000000000000000, 1.000000000000000000, 1.000000000000000000, 1.000000000000000000, 1.000000000000000000, 1.000000000000000000, 1.000000000000000000, 1.000000000000000000, 1.000000000000000000, 1.000000000000000000, 1.000000000000000000, 1.000000000000000000, 1.000000000000000000, 1.000000000000000000, 1.000000000000000000, 1.000000000000000000, 1.000000000000000000, 1.000000000000000000, 1.000000000000000000, 1.000000000000000000, 1.000000000000000000, 1.000000000000000000, 1.000000000000000000, 1.000000000000000000, 1.000000000000000000, 1.000000000000000000, 1.000000000000000000, 1.000000000000000000, 1.000000000000000000, 1.000000000000000000, 1.000000000000000000, 1.000000000000000000, 1.000000000000000000, 1.000000000000000000, 1.000000000000000000, 1.000000000000000000, 1.000000000000000000, 1.000000000000000000, 1.000000000000000000, 1.000000000000000000, 1.000000000000000000, 1.000000000000000000, 1.000000000000000000, 1.000000000000000000, 1.000000000000000000, 1.000000000000000000, 1.000000000000000000, 1.000000000000000000, 1.000000000000000000, 1.000000000000000000, 1.000000000000000000, 1.000000000000000000, 1.000000000000000000, 1.000000000000000000, 1.000000000000000000, 1.000000000000000000, 1.000000000000000000, 1.000000000000000000, 1.000000000000000000, 1.000000000000000000, 1.000000000000000000, 1.000000000000000000, 1.000000000000000000, 1.000000000000000000, 1.000000000000000000, 1.000000000000000000, 1.000000000000000000, 1.000000000000000000, 1.000000000000000000, 1.000000000000000000),
 ( 0.3333333333333333703, 0.3333333333333333703, 0.3333333333333333703, 0.3333333333333333703, 0.3333333333333333703, 0.3333333333333333703, 0.3333333333333333703, 0.3333333333333333703, 0.3333333333333333703, 0.3333333333333333703, 0.3333333333333333703, 0.3333333333333333703, 0.3333333333333333703, 0.3333333333333333703, 0.3333333333333333703, 0.3333333333333333703, 0.3333333333333333703, 0.3333333333333333703, 0.3333333333333333703, 0.3333333333333333703, 0.3333333333333333703, 0.3333333333333333703, 0.3333333333333333703, 0.3333333333333333703, 0.3333333333333333703, 0.3333333333333333703, 0.3333333333333333703, 0.3333333333333333703, 0.3333333333333333703, 0.3333333333333333703, 0.3333333333333333703, 0.3333333333333333703, 0.3333333333333333703, 0.3333333333333333703, 0.3333333333333333703, 0.3333333333333333703, 0.3333333333333333703, 0.3333333333333333703, 0.3333333333333333703, 0.3333333333333333703, 0.3333333333333333703, 0.3333333333333333703, 0.3333333333333333703, 0.3333333333333333703, 0.3333333333333333703, 0.3333333333333333703, 0.3333333333333333703, 0.3333333333333333703, 0.3333333333333333703, 0.3333333333333333703, 0.3333333333333333703, 0.3333333333333333703, 0.3333333333333333703, 0.3333333333333333703, 0.3333333333333333703, 0.3333333333333333703, 0.3333333333333333703, 0.3333333333333333703, 0.3333333333333333703, 0.3333333333333333703, 0.3333333333333333703, 0.3333333333333333703, 0.3333333333333333703, 0.3333333333333333703, 0.3333333333333333703, 0.3333333333333333703, 0.3333333333333333703, 0.3333333333333333703, 0.3333333333333333703, 0.3333333333333333703, 0.3333333333333333703, 0.3333333333333333703, 0.3333333333333333703, 0.3333333333333333703, 0.3333333333333333703, 0.3333333333333333703, 0.3333333333333333703, 0.3333333333333333703, 0.3333333333333333703, 0.3333333333333333703, 0.3333333333333333703, 0.3333333333333333703, 0.3333333333333333703, 0.3333333333333333703, 0.3333333333333333703, 0.3333333333333333703),
 ( 0.3333333333333333703, 0.3333333333333333703, 0.3333333333333333703, 0.3333333333333333703, 0.3333333333333333703, 0.3333333333333333703, 0.3333333333333333703, 0.3333333333333333703, 0.3333333333333333703, 0.3333333333333333703, 0.3333333333333333703, 0.3333333333333333703, 0.3333333333333333703, 0.3333333333333333703, 0.3333333333333333703, 0.3333333333333333703, 0.3333333333333333703, 0.3333333333333333703, 0.3333333333333333703, 0.3333333333333333703, 0.3333333333333333703, 0.3333333333333333703, 0.3333333333333333703, 0.3333333333333333703, 0.3333333333333333703, 0.3333333333333333703, 0.3333333333333333703, 0.3333333333333333703, 0.3333333333333333703, 0.3333333333333333703, 0.3333333333333333703, 0.3333333333333333703, 0.3333333333333333703, 0.3333333333333333703, 0.3333333333333333703, 0.3333333333333333703, 0.3333333333333333703, 0.3333333333333333703, 0.3333333333333333703, 0.3333333333333333703, 0.3333333333333333703, 0.3333333333333333703, 0.3333333333333333703, 0.3333333333333333703, 0.3333333333333333703, 0.3333333333333333703, 0.3333333333333333703, 0.3333333333333333703, 0.3333333333333333703, 0.3333333333333333703, 0.3333333333333333703, 0.3333333333333333703, 0.3333333333333333703, 0.3333333333333333703, 0.3333333333333333703, 0.3333333333333333703, 0.3333333333333333703, 0.3333333333333333703, 0.3333333333333333703, 0.3333333333333333703, 0.3333333333333333703, 0.3333333333333333703, 0.3333333333333333703, 0.3333333333333333703, 0.3333333333333333703, 0.3333333333333333703, 0.3333333333333333703, 0.3333333333333333703, 0.3333333333333333703, 0.3333333333333333703, 0.3333333333333333703, 0.3333333333333333703, 0.3333333333333333703, 0.3333333333333333703, 0.3333333333333333703, 0.3333333333333333703, 0.3333333333333333703, 0.3333333333333333703, 0.3333333333333333703, 0.3333333333333333703, 0.3333333333333333703, 0.3333333333333333703, 0.3333333333333333703, 0.3333333333333333703, 0.3333333333333333703, 0.3333333333333333703),
 ( 1.000000000000000000, 1.000000000000000000, 1.000000000000000000, 1.000000000000000000, 1.000000000000000000, 1.000000000000000000, 1.000000000000000000, 1.000000000000000000, 1.000000000000000000, 1.000000000000000000, 1.000000000000000000, 1.000000000000000000, 1.000000000000000000, 1.000000000000000000, 1.000000000000000000, 1.000000000000000000, 1.000000000000000000, 1.000000000000000000, 1.000000000000000000, 1.000000000000000000, 1.000000000000000000, 1.000000000000000000, 1.000000000000000000, 1.000000000000000000, 1.000000000000000000, 1.000000000000000000, 1.000000000000000000, 1.000000000000000000, 1.000000000000000000, 1.000000000000000000, 1.000000000000000000, 1.000000000000000000, 1.000000000000000000, 1.000000000000000000, 1.000000000000000000, 1.000000000000000000, 1.000000000000000000, 1.000000000000000000, 1.000000000000000000, 1.000000000000000000, 1.000000000000000000, 1.000000000000000000, 1.000000000000000000, 1.000000000000000000, 1.000000000000000000, 1.000000000000000000, 1.000000000000000000, 1.000000000000000000, 1.000000000000000000, 1.000000000000000000, 1.000000000000000000, 1.000000000000000000, 1.000000000000000000, 1.000000000000000000, 1.000000000000000000, 1.000000000000000000, 1.000000000000000000, 1.000000000000000000, 1.000000000000000000, 1.000000000000000000, 1.000000000000000000, 1.000000000000000000, 1.000000000000000000, 1.000000000000000000, 1.000000000000000000, 1.000000000000000000, 1.000000000000000000, 1.000000000000000000, 1.000000000000000000, 1.000000000000000000, 1.000000000000000000, 1.000000000000000000, 1.000000000000000000, 1.000000000000000000, 1.000000000000000000, 1.000000000000000000, 1.000000000000000000, 1.000000000000000000, 1.000000000000000000, 1.000000000000000000, 1.000000000000000000, 1.000000000000000000, 1.000000000000000000, 1.000000000000000000, 1.000000000000000000, 1.000000000000000000) ) ) 
 REPRESENTATION_ITEM ( '' )  SURFACE ( )  );
#8426 = LINE ( 'NONE', #11956, #2680 ) ;
#8427 = LINE ( 'NONE', #19520, #18675 ) ;
#8428 = CARTESIAN_POINT ( 'NONE',  ( -7.090308582316794173, -21.32581373872472597, 1.729004561291657582 ) ) ;
#8429 = CARTESIAN_POINT ( 'NONE',  ( -3.343476823822036259, -9.987837386737346890, 2.789442121235767402 ) ) ;
#8430 = ORIENTED_EDGE ( 'NONE', *, *, #18365, .T. ) ;
#8431 = CARTESIAN_POINT ( 'NONE',  ( -12.78345773956433895, -11.49788415197707181, 4.924178440007425550 ) ) ;
#8432 = CARTESIAN_POINT ( 'NONE',  ( -6.621558582316794173, -23.74999999999999645, 3.550687472877651629 ) ) ;
#8433 = CARTESIAN_POINT ( 'NONE',  ( -7.659691417683177406, -22.67418626127524917, 1.729004561291651809 ) ) ;
#8434 = VERTEX_POINT ( 'NONE', #8828 ) ;
#8435 = CARTESIAN_POINT ( 'NONE',  ( 13.83051420738022763, 3.503467472703414742, 5.232249963382380464 ) ) ;
#8436 = CARTESIAN_POINT ( 'NONE',  ( -20.00000000000000000, 3.000000000000000888, 1.500000000000000000 ) ) ;
#8437 = EDGE_LOOP ( 'NONE', ( #9586, #13334, #20512, #17372 ) ) ;
#8438 = ORIENTED_EDGE ( 'NONE', *, *, #3114, .T. ) ;
#8439 = AXIS2_PLACEMENT_3D ( 'NONE', #11443, #1821, #9666 ) ;
#8440 = ADVANCED_FACE ( 'NONE', ( #15193 ), #7050, .F. ) ;
#8441 = CARTESIAN_POINT ( 'NONE',  ( -27.94203811574921303, 11.64110105645932691, 0.000000000000000000 ) ) ;
#8442 = VERTEX_POINT ( 'NONE', #16553 ) ;
#8443 = CARTESIAN_POINT ( 'NONE',  ( -13.39482594849551944, -19.24878960097397140, 5.493002502378098839 ) ) ;
#8444 = ORIENTED_EDGE ( 'NONE', *, *, #18887, .T. ) ;
#8445 = CARTESIAN_POINT ( 'NONE',  ( 5.784691417683177406, -23.77099543870834353, 4.174186261275251830 ) ) ;
#8446 = CARTESIAN_POINT ( 'NONE',  ( 5.000000000000000000, -7.500000000000000000, 1.000000000000000000 ) ) ;
#8447 = EDGE_CURVE ( 'NONE', #10249, #16180, #14785, .T. ) ;
#8448 = CARTESIAN_POINT ( 'NONE',  ( 0.000000000000000000, 4.999999999999999112, 1.000000000000000000 ) ) ;
#8449 = LINE ( 'NONE', #4044, #1615 ) ;
#8450 = VECTOR ( 'NONE', #1083, 1000.000000000000000 ) ;
#8451 = LINE ( 'NONE', #11986, #1945 ) ;
#8452 = CARTESIAN_POINT ( 'NONE',  ( 7.847191417683176518, -21.22443879296941915, 1.770995438708345748 ) ) ;
#8453 = LINE ( 'NONE', #12835, #6885 ) ;
#8454 = CARTESIAN_POINT ( 'NONE',  ( -4.472191417683177406, -23.72900456129165292, 2.724438792969417822 ) ) ;
#8455 = CARTESIAN_POINT ( 'NONE',  ( -7.277808582316795061, -19.52099543870833642, 2.413778621189609286 ) ) ;
#8456 = VERTEX_POINT ( 'NONE', #8513 ) ;
#8457 = CARTESIAN_POINT ( 'NONE',  ( 12.62499979224180180, -20.25001049178813162, 4.458178821399696012 ) ) ;
#8458 = CARTESIAN_POINT ( 'NONE',  ( -13.14123030749026277, 5.069630528265579805, 6.418963484850015000 ) ) ;
#8459 = ORIENTED_EDGE ( 'NONE', *, *, #14847, .T. ) ;
#8460 = CARTESIAN_POINT ( 'NONE',  ( -9.689245429134309973, 11.64110105645932691, 0.000000000000000000 ) ) ;
#8461 = CARTESIAN_POINT ( 'NONE',  ( -9.999999999999996447, -34.99999999999999289, 1.000000000000000000 ) ) ;
#8462 = ORIENTED_EDGE ( 'NONE', *, *, #13307, .F. ) ;
#8463 = VERTEX_POINT ( 'NONE', #10083 ) ;
#8464 = VECTOR ( 'NONE', #2104, 1000.000000000000227 ) ;
#8465 = EDGE_CURVE ( 'NONE', #458, #510, #20023, .T. ) ;
#8466 = CARTESIAN_POINT ( 'NONE',  ( 12.66943601481756687, -20.06596378382619150, 3.544869486356359456 ) ) ;
#8467 = EDGE_LOOP ( 'NONE', ( #12493, #16157, #12641, #3870, #5865 ) ) ;
#8468 = CARTESIAN_POINT ( 'NONE',  ( 25.54469207716615031, 0.000000000000000000, 1.000000000000000000 ) ) ;
#8469 = CARTESIAN_POINT ( 'NONE',  ( 13.00900269284621302, -0.8578640112522492034, 5.903024842915844062 ) ) ;
#8470 = EDGE_CURVE ( 'NONE', #7956, #19341, #5476, .T. ) ;
#8471 = CARTESIAN_POINT ( 'NONE',  ( 0.000000000000000000, 16.00000000000000000, 1.000000000000000000 ) ) ;
#8472 = EDGE_CURVE ( 'NONE', #15081, #20661, #2029, .T. ) ;
#8473 = CARTESIAN_POINT ( 'NONE',  ( 12.63943061533661982, -19.52125392549825733, 5.470334935344855154 ) ) ;
#8474 = DIRECTION ( 'NONE',  ( -0.1736481776669295263, -0.9848077530122082424, 0.000000000000000000 ) ) ;
#8475 = CARTESIAN_POINT ( 'NONE',  ( 11.21530858231679595, -24.52099543870834708, 2.515153566944913432 ) ) ;
#8476 = CARTESIAN_POINT ( 'NONE',  ( -12.62499979224180180, -20.25001049178813162, 4.458178821399696012 ) ) ;
#8477 = CARTESIAN_POINT ( 'NONE',  ( -6.902808582316795949, -23.08622137881038938, 1.020995438708339309 ) ) ;
#8478 = DIRECTION ( 'NONE',  ( 1.000000000000000000, 0.000000000000000000, -0.000000000000000000 ) ) ;
#8479 = PLANE ( 'NONE',  #3740 ) ;
#8480 = CARTESIAN_POINT ( 'NONE',  ( 9.152808582316795949, -21.53509896474924901, 4.479004561291659137 ) ) ;
#8481 = CARTESIAN_POINT ( 'NONE',  ( -7.940941417683176518, -20.72672167713052715, 2.298404588716546293 ) ) ;
#8482 = ORIENTED_EDGE ( 'NONE', *, *, #11405, .T. ) ;
#8483 = ORIENTED_EDGE ( 'NONE', *, *, #6918, .T. ) ;
#8484 = CARTESIAN_POINT ( 'NONE',  ( 13.41341218697771609, -18.31018455762212227, 5.513179699623425023 ) ) ;
#8485 = DIRECTION ( 'NONE',  ( 1.000000000000000000, 0.000000000000000000, -0.000000000000000000 ) ) ;
#8486 = DIRECTION ( 'NONE',  ( 0.000000000000000000, 0.000000000000000000, 1.000000000000000000 ) ) ;
#8487 = ORIENTED_EDGE ( 'NONE', *, *, #17457, .T. ) ;
#8488 = EDGE_CURVE ( 'NONE', #19095, #5490, #2913, .T. ) ;
#8489 = FACE_OUTER_BOUND ( 'NONE', #13544, .T. ) ;
#8490 = FACE_OUTER_BOUND ( 'NONE', #9251, .T. ) ;
#8491 = CARTESIAN_POINT ( 'NONE',  ( 14.50000000000000000, -23.00000000000001421, 4.000000000000000000 ) ) ;
#8492 = CARTESIAN_POINT ( 'NONE',  ( 13.39662663169496781, -19.15785509940297615, 5.494950532956567102 ) ) ;
#8493 = LINE ( 'NONE', #12141, #842 ) ;
#8494 = CARTESIAN_POINT ( 'NONE',  ( 1.884282074604925583, -8.375506800461993251, 2.375363417140690547 ) ) ;
#8495 = LINE ( 'NONE', #14864, #6050 ) ;
#8496 = CARTESIAN_POINT ( 'NONE',  ( -12.62503976493681535, -19.49799187068907713, 4.533161381885315144 ) ) ;
#8497 = CARTESIAN_POINT ( 'NONE',  ( 5.496558582316794173, -22.05068747287764452, 1.749999999999998446 ) ) ;
#8498 = LINE ( 'NONE', #14965, #14063 ) ;
#8499 = CARTESIAN_POINT ( 'NONE',  ( 12.66849571425264287, -18.05346643024382303, 5.533233176248494978 ) ) ;
#8500 = CARTESIAN_POINT ( 'NONE',  ( -1.904508877737772998, -9.138371295333994837, 2.378667276417936627 ) ) ;
#8501 = CARTESIAN_POINT ( 'NONE',  ( 8.684058582316795949, -21.32873467460644079, 2.757051763020455404 ) ) ;
#8502 = CARTESIAN_POINT ( 'NONE',  ( 10.47219141768317563, -23.72900456129165292, 2.724438792969417822 ) ) ;
#8503 = CARTESIAN_POINT ( 'NONE',  ( -9.902808582316795949, -22.46490103525074034, 2.520995438708341307 ) ) ;
#8504 = ORIENTED_EDGE ( 'NONE', *, *, #545, .T. ) ;
#8505 = CARTESIAN_POINT ( 'NONE',  ( 12.63806878948643231, -20.34002613093225520, 5.891296472647073124 ) ) ;
#8506 = CARTESIAN_POINT ( 'NONE',  ( 12.63118877378512828, -19.18746692385052555, 4.758813856674282583 ) ) ;
#8507 = CARTESIAN_POINT ( 'NONE',  ( -14.00000000000000000, 0.000000000000000000, 2.000000000000000000 ) ) ;
#8508 = ORIENTED_EDGE ( 'NONE', *, *, #5199, .T. ) ;
#8509 = ADVANCED_FACE ( 'NONE', ( #18031 ), #2130, .T. ) ;
#8510 = ORIENTED_EDGE ( 'NONE', *, *, #11576, .F. ) ;
#8511 = EDGE_CURVE ( 'NONE', #1283, #15113, #18239, .T. ) ;
#8512 = FACE_OUTER_BOUND ( 'NONE', #8212, .T. ) ;
#8513 = CARTESIAN_POINT ( 'NONE',  ( 10.49999999999999645, -9.999999999999991118, 2.500000000000000000 ) ) ;
#8514 = DIRECTION ( 'NONE',  ( 0.000000000000000000, 0.000000000000000000, 1.000000000000000000 ) ) ;
#8515 = DIRECTION ( 'NONE',  ( 0.000000000000000000, 1.000000000000000000, 0.000000000000000000 ) ) ;
#8516 = CARTESIAN_POINT ( 'NONE',  ( 1.668644041176298387, -9.864915931696323526, 2.372643470467795890 ) ) ;
#8517 = LINE ( 'NONE', #9977, #47 ) ;
#8518 = CARTESIAN_POINT ( 'NONE',  ( 17.30017143803810242, 0.000000000000000000, 0.000000000000000000 ) ) ;
#8519 = EDGE_CURVE ( 'NONE', #3752, #10986, #17266, .T. ) ;
#8520 = CARTESIAN_POINT ( 'NONE',  ( 3.747260319564023501, 9.000000000000001776, 1.000000000000000000 ) ) ;
#8521 = CARTESIAN_POINT ( 'NONE',  ( -2.513306525444908512, -9.622685169956881168, 2.503048754562789746 ) ) ;
#8522 = CARTESIAN_POINT ( 'NONE',  ( -5.965308582316793284, -20.22900456129164937, 4.174186261275266929 ) ) ;
#8523 = CARTESIAN_POINT ( 'NONE',  ( -0.5631383031621635116, -8.364917468222230923, 2.372643865078341019 ) ) ;
#8524 = ORIENTED_EDGE ( 'NONE', *, *, #4414, .T. ) ;
#8525 = CARTESIAN_POINT ( 'NONE',  ( -13.64827103573800571, -5.699812695207630675, 5.034333296717131034 ) ) ;
#8526 = CARTESIAN_POINT ( 'NONE',  ( -4.746558582316793284, -21.94931252712234482, 5.250000000000000888 ) ) ;
#8527 = CARTESIAN_POINT ( 'NONE',  ( -9.909691417683179182, -21.32581373872474373, 5.270995438708348857 ) ) ;
#8528 = ORIENTED_EDGE ( 'NONE', *, *, #11089, .F. ) ;
#8529 = CARTESIAN_POINT ( 'NONE',  ( 13.84501469867365131, 4.235742283194553259, 3.333333333332063386 ) ) ;
#8531 = CARTESIAN_POINT ( 'NONE',  ( -17.55017143803810242, 9.000000000000001776, 1.000000000000000000 ) ) ;
#8530 = AXIS2_PLACEMENT_3D ( 'NONE', #10368, #3881, #20107 ) ;
#8532 = VERTEX_POINT ( 'NONE', #20128 ) ;
#8533 = ORIENTED_EDGE ( 'NONE', *, *, #10567, .T. ) ;
#8534 = LINE ( 'NONE', #269, #11726 ) ;
#8535 = VERTEX_POINT ( 'NONE', #9029 ) ;
#8536 = CARTESIAN_POINT ( 'NONE',  ( -13.37500000000002132, -20.25000000000274269, 4.083333333315724012 ) ) ;
#8537 = B_SPLINE_CURVE_WITH_KNOTS ( 'NONE', 3,
 ( #16349, #3490, #16250, #1919, #10078, #16452, #19703, #2126, #14878, #11743 ),
 .UNSPECIFIED., .F., .F.,
 ( 4, 2, 2, 2, 4 ),
 ( 0.001177954577779514490, 0.001472373510017591655, 0.001766792442255668821, 0.002061211374493746203, 0.002355630306731823151 ),
 .UNSPECIFIED. ) ;
#8538 = ORIENTED_EDGE ( 'NONE', *, *, #528, .F. ) ;
#8539 = CARTESIAN_POINT ( 'NONE',  ( 3.944195004867014909, -21.61378581760806128, 5.207602947182413011 ) ) ;
#8540 = LINE ( 'NONE', #13142, #14657 ) ;
#8541 = CARTESIAN_POINT ( 'NONE',  ( 5.999999999999999112, -7.500000000000047073, 9.999999999999998224 ) ) ;
#8542 = CARTESIAN_POINT ( 'NONE',  ( 3.343476823822036259, -9.987837386737346890, 2.789442121235767402 ) ) ;
#8543 = CARTESIAN_POINT ( 'NONE',  ( -6.527808582316794173, -23.72900456129165292, 4.275561207030568411 ) ) ;
#8544 = EDGE_CURVE ( 'NONE', #10614, #12628, #8392, .T. ) ;
#8545 = CARTESIAN_POINT ( 'NONE',  ( 12.65346245025441263, -19.56264626215117275, 6.228892365149262922 ) ) ;
#8546 = CARTESIAN_POINT ( 'NONE',  ( 15.00000000000000000, 3.673940397442059178E-15, 2.000000000000000000 ) ) ;
#8547 = CARTESIAN_POINT ( 'NONE',  ( 9.534691417683177406, -20.22900456129164581, 2.825813738724747726 ) ) ;
#8548 = CARTESIAN_POINT ( 'NONE',  ( -20.92243175760212637, 0.000000000000000000, 0.000000000000000000 ) ) ;
#8549 = CARTESIAN_POINT ( 'NONE',  ( -4.847191417683177406, -21.53509896474923835, 2.520995438708346192 ) ) ;
#8550 = CARTESIAN_POINT ( 'NONE',  ( -6.809058582316796837, -23.80360840875935935, 1.768074502826626260 ) ) ;
#8551 = ORIENTED_EDGE ( 'NONE', *, *, #11089, .T. ) ;
#8552 = CARTESIAN_POINT ( 'NONE',  ( 12.62500016093973620, -20.24999187254239175, 4.532396751752561848 ) ) ;
#8553 = CARTESIAN_POINT ( 'NONE',  ( -12.62499999999998579, -20.24999999999999289, 3.666666666666653640 ) ) ;
#8554 = ORIENTED_EDGE ( 'NONE', *, *, #16038, .F. ) ;
#8555 = PLANE ( 'NONE',  #15959 ) ;
#8556 = FACE_OUTER_BOUND ( 'NONE', #9738, .T. ) ;
#8557 = ORIENTED_EDGE ( 'NONE', *, *, #293, .T. ) ;
#8558 = PRODUCT_RELATED_PRODUCT_CATEGORY ( 'part', '', ( #18864 ) ) ;
#8559 = APPLICATION_PROTOCOL_DEFINITION ( 'draft international standard', 'automotive_design', 1998, #6151 ) ;
#8560 = ORIENTED_EDGE ( 'NONE', *, *, #7980, .F. ) ;
#8561 = CARTESIAN_POINT ( 'NONE',  ( 13.33984198047847514, -20.08950154656911380, 3.453859469323321552 ) ) ;
#8562 = VERTEX_POINT ( 'NONE', #14338 ) ;
#8563 = DIRECTION ( 'NONE',  ( 0.000000000000000000, -1.000000000000000000, 0.000000000000000000 ) ) ;
#8564 = CARTESIAN_POINT ( 'NONE',  ( 13.12529397354238192, 5.014845663890295846, 4.166666666666749563 ) ) ;
#8565 = CARTESIAN_POINT ( 'NONE',  ( -1.819865260185086875, -9.122006307963404836, 1.624464420737683046 ) ) ;
#8566 = LINE ( 'NONE', #12778, #10018 ) ;
#8567 = CARTESIAN_POINT ( 'NONE',  ( 5.683390479346035029, 4.999999999999999112, 1.000000000000000000 ) ) ;
#8568 = CARTESIAN_POINT ( 'NONE',  ( 13.12529397354238192, 5.014845663890295846, 3.666666666666500873 ) ) ;
#8569 = CARTESIAN_POINT ( 'NONE',  ( 4.687312169500631676, -21.54001800463478133, 5.087297191110758732 ) ) ;
#8570 = VECTOR ( 'NONE', #9774, 1000.000000000000000 ) ;
#8571 = CARTESIAN_POINT ( 'NONE',  ( 10.84030858231679595, -22.98484643305508612, 6.020995438708344416 ) ) ;
#8572 = CARTESIAN_POINT ( 'NONE',  ( -13.11465082267961968, 3.727366545318180791, 6.751662912489328150 ) ) ;
#8573 = CARTESIAN_POINT ( 'NONE',  ( -8.222191417683175629, -19.52099543870834353, 4.586221378810406257 ) ) ;
#8574 = EDGE_CURVE ( 'NONE', #11223, #12439, #1900, .T. ) ;
#8575 = CARTESIAN_POINT ( 'NONE',  ( -30.00000000000000000, 10.00000000000000000, 1.000000000000000000 ) ) ;
#8576 = DIRECTION ( 'NONE',  ( 1.000000000000000000, 0.000000000000000000, 0.000000000000000000 ) ) ;
#8577 = CARTESIAN_POINT ( 'NONE',  ( 7.934058582316796837, -22.67126532539354855, 4.242948236979545484 ) ) ;
#8578 = LINE ( 'NONE', #627, #4319 ) ;
#8579 = EDGE_LOOP ( 'NONE', ( #6634, #17065, #9094, #7435, #18976, #454, #6455, #3433, #5369, #13586, #3516, #18542, #10198, #17354, #20515, #12023, #3308, #14592, #4263, #5785, #15576, #14979, #15758, #19305, #10976, #20508, #10587, #1031, #10960, #2431, #4688, #2247, #8158, #11869, #11359, #13433, #17317, #1559, #17747, #1745, #3310, #15566, #5188, #18724, #10080, #10487, #5884, #9995, #20648, #12632, #16550, #20388, #6351, #17940, #13058, #19768, #1536, #2342, #17320, #18892, #12171, #6405, #1766, #1749, #16478, #7194, #4674, #15621, #11688, #1387, #8232, #16573, #19174, #17479, #20344, #19841, #6188, #2174, #14207, #10253, #6484, #11485, #17268, #12868, #18528, #15319, #18886, #16934, #14782, #767, #10778, #9128, #12920, #16916, #19914, #10568, #12134, #10858, #11301, #3847, #14676, #13657, #11210, #7301, #19740, #18311, #16912, #4943, #14852, #15287, #19301, #3492, #8896, #11430, #10178, #2588, #10544, #9191, #2502, #10982 ) ) ;
#8580 = ORIENTED_EDGE ( 'NONE', *, *, #9922, .T. ) ;
#8581 = CARTESIAN_POINT ( 'NONE',  ( 13.87066368810231154, 4.781016249162736820, 5.617237349937618696 ) ) ;
#8582 = ADVANCED_FACE ( 'NONE', ( #15909 ), #1799, .F. ) ;
#8583 = CARTESIAN_POINT ( 'NONE',  ( -19.48630159782011262, 4.999999999999999112, 1.000000000000000000 ) ) ;
#8584 = FILL_AREA_STYLE_COLOUR ( '', #17361 ) ;
#8585 = EDGE_LOOP ( 'NONE', ( #4205, #16857, #18515, #16958 ) ) ;
#8586 = LINE ( 'NONE', #5451, #20150 ) ;
#8587 = LINE ( 'NONE', #14955, #1029 ) ;
#8588 = LINE ( 'NONE', #18425, #10984 ) ;
#8589 = CARTESIAN_POINT ( 'NONE',  ( 13.85788212999909419, 4.135547564954428879, 5.982801014393342776 ) ) ;
#8590 = DIRECTION ( 'NONE',  ( 0.000000000000000000, 0.000000000000000000, -1.000000000000000000 ) ) ;
#8591 = CARTESIAN_POINT ( 'NONE',  ( 0.2815691515810352374, -8.364917468222230923, 2.372643865078523540 ) ) ;
#8592 = CARTESIAN_POINT ( 'NONE',  ( -21.42243175760212637, 4.999999999999999112, 1.000000000000000000 ) ) ;
#8593 = CARTESIAN_POINT ( 'NONE',  ( -13.06641424290328501, 2.791419266617020334, 5.231470106674447784 ) ) ;
#8594 = CARTESIAN_POINT ( 'NONE',  ( 6.152808582316794173, -21.22443879296942626, 5.229004561291660025 ) ) ;
#8595 = CARTESIAN_POINT ( 'NONE',  ( -19.48630159782011262, 9.000000000000001776, 1.000000000000000000 ) ) ;
#8596 = CARTESIAN_POINT ( 'NONE',  ( 13.12526104302547836, 5.013182672784613381, 5.066812735559260261 ) ) ;
#8597 = ADVANCED_FACE ( 'NONE', ( #130 ), #11311, .F. ) ;
#8598 = CARTESIAN_POINT ( 'NONE',  ( -0.9854920305337621089, -9.114917468222230923, 2.372643865078341019 ) ) ;
#8599 = CARTESIAN_POINT ( 'NONE',  ( 10.84030858231679595, -22.36352608949544418, 4.520995438708343528 ) ) ;
#8600 = AXIS2_PLACEMENT_3D ( 'NONE', #15481, #20418, #15269 ) ;
#8601 = CARTESIAN_POINT ( 'NONE',  ( 7.190941417683176518, -23.27327832286946219, 4.701595411283453707 ) ) ;
#8602 = CARTESIAN_POINT ( 'NONE',  ( -9.434058582316794173, -23.20159541128345992, 4.773278322869455970 ) ) ;
#8603 = ORIENTED_EDGE ( 'NONE', *, *, #14717, .F. ) ;
#8604 = CARTESIAN_POINT ( 'NONE',  ( 12.70700162295422864, -16.85891804079483691, 6.308954579156044851 ) ) ;
#8605 = ADVANCED_FACE ( 'NONE', ( #14654 ), #11012, .F. ) ;
#8606 = CARTESIAN_POINT ( 'NONE',  ( 12.93692567357942202, -3.747753484270499591, 5.090845106672844622 ) ) ;
#8607 = EDGE_CURVE ( 'NONE', #14781, #5093, #14230, .T. ) ;
#8608 = DIRECTION ( 'NONE',  ( 0.000000000000000000, 0.000000000000000000, 1.000000000000000000 ) ) ;
#8609 = ORIENTED_EDGE ( 'NONE', *, *, #15120, .F. ) ;
#8610 = ORIENTED_EDGE ( 'NONE', *, *, #13196, .F. ) ;
#8611 = LINE ( 'NONE', #11848, #19821 ) ;
#8612 = ADVANCED_FACE ( 'NONE', ( #4617 ), #3261, .T. ) ;
#8613 = PLANE ( 'NONE',  #15921 ) ;
#8614 = DIRECTION ( 'NONE',  ( -0.000000000000000000, 0.000000000000000000, -1.000000000000000000 ) ) ;
#8615 = CARTESIAN_POINT ( 'NONE',  ( -3.944195004867014909, -21.58936506995667770, 5.302691919372072960 ) ) ;
#8616 = CARTESIAN_POINT ( 'NONE',  ( 1.743623630681728542, -9.116095536440919744, 2.372946416531167557 ) ) ;
#8617 = DIRECTION ( 'NONE',  ( 0.000000000000000000, 1.000000000000000000, -0.000000000000000000 ) ) ;
#8618 = DIRECTION ( 'NONE',  ( -0.000000000000000000, -0.000000000000000000, -1.000000000000000000 ) ) ;
#8619 = AXIS2_PLACEMENT_3D ( 'NONE', #6578, #12943, #19346 ) ;
#8620 = EDGE_CURVE ( 'NONE', #17290, #13360, #9439, .T. ) ;
#8621 = CARTESIAN_POINT ( 'NONE',  ( 0.000000000000000000, 9.000000000000001776, 1.000000000000000000 ) ) ;
#8622 = DIRECTION ( 'NONE',  ( 0.000000000000000000, 0.000000000000000000, -1.000000000000000000 ) ) ;
#8623 = CARTESIAN_POINT ( 'NONE',  ( -9.621558582316794173, -23.74999999999999645, 3.550687472877651629 ) ) ;
#8624 = ADVANCED_FACE ( 'NONE', ( #1701 ), #14448, .T. ) ;
#8625 = CARTESIAN_POINT ( 'NONE',  ( -3.173374397671306912, -9.279487642487616483, 2.607523756204581211 ) ) ;
#8626 = VERTEX_POINT ( 'NONE', #6411 ) ;
#8627 = CARTESIAN_POINT ( 'NONE',  ( -13.09560264575884503, 4.265433610975056133, 3.333333333333364568 ) ) ;
#8628 = CARTESIAN_POINT ( 'NONE',  ( -4.934058582316793284, -23.20159541128345992, 4.773278322869455970 ) ) ;
#8629 = CARTESIAN_POINT ( 'NONE',  ( -8.690941417683177406, -23.27327832286946219, 4.701595411283453707 ) ) ;
#8630 = ORIENTED_EDGE ( 'NONE', *, *, #15176, .F. ) ;
#8631 = CARTESIAN_POINT ( 'NONE',  ( 13.84504075139246915, 3.487057945321567765, 5.981929699623240282 ) ) ;
#8632 = PLANE ( 'NONE',  #9711 ) ;
#8633 = VERTEX_POINT ( 'NONE', #12775 ) ;
#8634 = ORIENTED_EDGE ( 'NONE', *, *, #19862, .F. ) ;
#8635 = CARTESIAN_POINT ( 'NONE',  ( 14.50000000000001243, -18.49999999999999645, 4.000000000000000000 ) ) ;
#8636 = VECTOR ( 'NONE', #9592, 1000.000000000000000 ) ;
#8637 = ORIENTED_EDGE ( 'NONE', *, *, #14119, .T. ) ;
#8638 = CARTESIAN_POINT ( 'NONE',  ( -13.37561105820882013, -20.21914156045197686, 4.753815841436231260 ) ) ;
#8639 = ORIENTED_EDGE ( 'NONE', *, *, #18109, .F. ) ;
#8640 = CARTESIAN_POINT ( 'NONE',  ( 6.253441417683176518, -21.94931252712233061, 1.749999999999998446 ) ) ;
#8641 = DIRECTION ( 'NONE',  ( -1.000000000000000000, 4.625929269271477434E-15, 0.000000000000000000 ) ) ;
#8642 = CARTESIAN_POINT ( 'NONE',  ( -13.87470602645761808, 4.985154336109792972, 4.000000000000000000 ) ) ;
#8643 = CARTESIAN_POINT ( 'NONE',  ( 3.996922828336520794, -14.62728872172488437, 3.980945906412841850 ) ) ;
#8644 = CARTESIAN_POINT ( 'NONE',  ( -7.652808582316794173, -21.22443879296942626, 5.229004561291660025 ) ) ;
#8645 = EDGE_CURVE ( 'NONE', #2799, #13818, #19179, .T. ) ;
#8646 = CARTESIAN_POINT ( 'NONE',  ( 12.62608183053121458, -20.94536755816881168, 4.949360998036265613 ) ) ;
#8647 = VECTOR ( 'NONE', #7571, 1000.000000000000000 ) ;
#8648 = CARTESIAN_POINT ( 'NONE',  ( 5.999999999999999112, -7.500000000000047073, 9.999999999999998224 ) ) ;
#8649 = EDGE_CURVE ( 'NONE', #8562, #17561, #16132, .T. ) ;
#8650 = CARTESIAN_POINT ( 'NONE',  ( 4.940941417683177406, -20.72672167713052715, 2.298404588716546293 ) ) ;
#8651 = CARTESIAN_POINT ( 'NONE',  ( -12.62499999999998224, -20.24999999999998934, 4.291666666666698937 ) ) ;
#8652 = CARTESIAN_POINT ( 'NONE',  ( -5.503441417683177406, -22.05068747287766229, 4.499999999999999112 ) ) ;
#8653 = CARTESIAN_POINT ( 'NONE',  ( -5.777808582316795949, -19.52099543870833642, 2.413778621189609286 ) ) ;
#8654 = EDGE_LOOP ( 'NONE', ( #10174, #12692, #20248, #13140 ) ) ;
#8655 = CARTESIAN_POINT ( 'NONE',  ( 13.12529397354238192, 5.014845663890295846, 4.833333333333344584 ) ) ;
#8656 = CARTESIAN_POINT ( 'NONE',  ( -12.64511805349267526, -19.23403829861753422, 5.507852591554869726 ) ) ;
#8657 = VERTEX_POINT ( 'NONE', #2616 ) ;
#8658 = CARTESIAN_POINT ( 'NONE',  ( 7.619520639128047002, 0.000000000000000000, 1.000000000000000000 ) ) ;
#8659 = DIRECTION ( 'NONE',  ( -0.1736481776669295540, 0.9848077530122082424, 0.000000000000000000 ) ) ;
#8660 = ORIENTED_EDGE ( 'NONE', *, *, #13815, .F. ) ;
#8661 = VECTOR ( 'NONE', #7898, 1000.000000000000000 ) ;
#8662 = CONTEXT_DEPENDENT_SHAPE_REPRESENTATION ( #19108, #11349 ) ;
#8663 = VERTEX_POINT ( 'NONE', #5661 ) ;
#8664 = ADVANCED_FACE ( 'NONE', ( #10678 ), #17051, .T. ) ;
#8665 = AXIS2_PLACEMENT_3D ( 'NONE', #11891, #16703, #3845 ) ;
#8666 = DIRECTION ( 'NONE',  ( 0.000000000000000000, 1.000000000000000000, -0.000000000000000000 ) ) ;
#8667 = ORIENTED_EDGE ( 'NONE', *, *, #8447, .T. ) ;
#8668 = DIRECTION ( 'NONE',  ( 0.000000000000000000, -0.2487476929738665354, -0.9685683172808094987 ) ) ;
#8669 = CARTESIAN_POINT ( 'NONE',  ( 12.79798428357658047, -11.51429367935891790, 5.673858176248284479 ) ) ;
#8670 = CARTESIAN_POINT ( 'NONE',  ( -2.739050625766161762, -9.875938058683834342, 1.818089155622620412 ) ) ;
#8671 = LINE ( 'NONE', #16601, #9982 ) ;
#8672 = CARTESIAN_POINT ( 'NONE',  ( -0.000000000000000000, 10.00000000000000000, 0.000000000000000000 ) ) ;
#8673 = LINE ( 'NONE', #1121, #13084 ) ;
#8674 = DIRECTION ( 'NONE',  ( -1.000000000000000000, -0.000000000000000000, -0.000000000000000000 ) ) ;
#8675 = AXIS2_PLACEMENT_3D ( 'NONE', #10210, #8641, #19540 ) ;
#8676 = CARTESIAN_POINT ( 'NONE',  ( 10.94094141768317741, -20.19639159124061933, 1.768074502826635586 ) ) ;
#8677 = CARTESIAN_POINT ( 'NONE',  ( -13.12529397354238192, 5.014845663890295846, 4.916666666666650087 ) ) ;
#8678 = CARTESIAN_POINT ( 'NONE',  ( -5.972191417683178294, -24.47900456129165292, 2.413778621189595963 ) ) ;
#8679 = VECTOR ( 'NONE', #14978, 1000.000000000000000 ) ;
#8680 = VERTEX_POINT ( 'NONE', #15581 ) ;
#8681 = FACE_OUTER_BOUND ( 'NONE', #127, .T. ) ;
#8682 = DIRECTION ( 'NONE',  ( 0.000000000000000000, -1.000000000000000000, 0.000000000000000000 ) ) ;
#8683 = CARTESIAN_POINT ( 'NONE',  ( -13.83065313257865370, 2.760483195222930952, 5.966304699623404595 ) ) ;
#8684 = CIRCLE ( 'NONE', #10355, 1.499999999999998668 ) ;
#8685 = CARTESIAN_POINT ( 'NONE',  ( 10.18405858231679595, -21.32873467460644079, 2.757051763020455404 ) ) ;
#8686 = CARTESIAN_POINT ( 'NONE',  ( 4.687312169500630787, -21.51559725698340131, 5.182386163300424009 ) ) ;
#8687 = VERTEX_POINT ( 'NONE', #17251 ) ;
#8688 = EDGE_LOOP ( 'NONE', ( #6878, #14851, #18908, #1505, #8899, #14726, #14445, #8965 ) ) ;
#8689 = CARTESIAN_POINT ( 'NONE',  ( 13.86693669322925260, 4.592803008081209448, 5.801483467520450077 ) ) ;
#8690 = DIRECTION ( 'NONE',  ( -0.000000000000000000, -0.000000000000000000, -1.000000000000000000 ) ) ;
#8691 = ORIENTED_EDGE ( 'NONE', *, *, #10521, .F. ) ;
#8692 = LINE ( 'NONE', #5236, #4111 ) ;
#8693 = CARTESIAN_POINT ( 'NONE',  ( 18.44064177244175440, 10.00000000000000000, 0.000000000000000000 ) ) ;
#8694 = CARTESIAN_POINT ( 'NONE',  ( 5.683390479346035029, 9.000000000000001776, 0.000000000000000000 ) ) ;
#8695 = EDGE_CURVE ( 'NONE', #5420, #14753, #10476, .T. ) ;
#8696 = CARTESIAN_POINT ( 'NONE',  ( 13.38238173943565990, -19.87722215849730034, 5.285856107751903288 ) ) ;
#8697 = CARTESIAN_POINT ( 'NONE',  ( -26.94203811574920593, 16.00000000000000000, 1.000000000000000000 ) ) ;
#8698 = CARTESIAN_POINT ( 'NONE',  ( 1.643076795806035717, -8.364903549957356077, 2.372640290589878909 ) ) ;
#8699 = AXIS2_PLACEMENT_3D ( 'NONE', #129, #13088, #11419 ) ;
#8700 = LINE ( 'NONE', #7139, #9063 ) ;
#8701 = CARTESIAN_POINT ( 'NONE',  ( -12.62499999999998224, -19.49999999999991473, 4.333333333333343695 ) ) ;
#8702 =( LENGTH_UNIT ( ) NAMED_UNIT ( * ) SI_UNIT ( .MILLI., .METRE. ) );
#8703 = PLANE ( 'NONE',  #13067 ) ;
#8704 = CARTESIAN_POINT ( 'NONE',  ( 12.64511805349267526, -19.23403829861753422, 5.507852591554869726 ) ) ;
#8705 = CARTESIAN_POINT ( 'NONE',  ( -2.436080212393455735, -9.483920418190111334, 2.467411194204634839 ) ) ;
#8706 = CARTESIAN_POINT ( 'NONE',  ( 10.65280858231679595, -21.53509896474924901, 4.479004561291659137 ) ) ;
#8707 = CARTESIAN_POINT ( 'NONE',  ( 10.94094141768317741, -20.72672167713052715, 2.298404588716546293 ) ) ;
#8708 = CARTESIAN_POINT ( 'NONE',  ( -7.746558582316794173, -21.94931252712234482, 5.250000000000000888 ) ) ;
#8709 = AXIS2_PLACEMENT_3D ( 'NONE', #1870, #6687, #11184 ) ;
#8710 = ORIENTED_EDGE ( 'NONE', *, *, #5137, .F. ) ;
#8711 = CARTESIAN_POINT ( 'NONE',  ( 13.15469878640066526, 5.749788713235649773, 5.232478742873432509 ) ) ;
#8712 = CARTESIAN_POINT ( 'NONE',  ( 13.08439876642066935, 3.699637704240349656, 5.251001356674258602 ) ) ;
#8713 = PLANE ( 'NONE',  #7341 ) ;
#8714 = VECTOR ( 'NONE', #15730, 1000.000000000000000 ) ;
#8715 = ORIENTED_EDGE ( 'NONE', *, *, #4677, .F. ) ;
#8716 = VECTOR ( 'NONE', #1297, 1000.000000000000000 ) ;
#8717 = VECTOR ( 'NONE', #7468, 1000.000000000000227 ) ;
#8718 = VERTEX_POINT ( 'NONE', #2834 ) ;
#8719 = FACE_OUTER_BOUND ( 'NONE', #7960, .T. ) ;
#8720 = CIRCLE ( 'NONE', #11388, 10.00000000000000000 ) ;
#8721 = EDGE_CURVE ( 'NONE', #15336, #20292, #5768, .T. ) ;
#8722 = CARTESIAN_POINT ( 'NONE',  ( 11.49178095869207006, 0.000000000000000000, 0.000000000000000000 ) ) ;
#8723 = LINE ( 'NONE', #15093, #9984 ) ;
#8724 = ADVANCED_FACE ( 'NONE', ( #19997 ), #7231, .T. ) ;
#8725 = LINE ( 'NONE', #773, #12328 ) ;
#8726 = CARTESIAN_POINT ( 'NONE',  ( 2.645259258103298983, -10.28229522185712241, 2.672449792925449596 ) ) ;
#8727 = CARTESIAN_POINT ( 'NONE',  ( 12.25209451496117197, 11.64110105645932691, 10.00000000000000000 ) ) ;
#8728 = VECTOR ( 'NONE', #20530, 1000.000000000000000 ) ;
#8729 = EDGE_CURVE ( 'NONE', #4492, #16474, #14011, .T. ) ;
#8730 = CARTESIAN_POINT ( 'NONE',  ( 5.999999999999999112, -2.500000000000047518, 9.999999999999998224 ) ) ;
#8731 = VECTOR ( 'NONE', #3477, 1000.000000000000000 ) ;
#8732 = CARTESIAN_POINT ( 'NONE',  ( 6.813547257480585095, 10.00000000000000000, 0.000000000000000000 ) ) ;
#8733 = FACE_OUTER_BOUND ( 'NONE', #7041, .T. ) ;
#8734 = CARTESIAN_POINT ( 'NONE',  ( -5.027808582316793284, -23.72900456129165647, 4.275561207030568411 ) ) ;
#8735 = CARTESIAN_POINT ( 'NONE',  ( -3.594802210173583035, -11.77224174634763898, 3.247712807842289884 ) ) ;
#8736 = ORIENTED_EDGE ( 'NONE', *, *, #19153, .T. ) ;
#8737 = CARTESIAN_POINT ( 'NONE',  ( -13.09560264576187905, 4.265433610975056133, 2.999999999999999556 ) ) ;
#8738 = CARTESIAN_POINT ( 'NONE',  ( -7.840308582316794173, -22.67418626127525982, 5.270995438708342640 ) ) ;
#8739 = CARTESIAN_POINT ( 'NONE',  ( 7.746558582316795949, -21.94931252712234127, 6.000000000000001776 ) ) ;
#8740 = CARTESIAN_POINT ( 'NONE',  ( -7.472191417683177406, -22.97900456129165292, 3.035098964749240125 ) ) ;
#8741 = ORIENTED_EDGE ( 'NONE', *, *, #1948, .F. ) ;
#8742 = CARTESIAN_POINT ( 'NONE',  ( 13.40382044110196347, -18.79456772435387890, 5.502763032956559108 ) ) ;
#8743 = CARTESIAN_POINT ( 'NONE',  ( -20.00000000000000000, 0.000000000000000000, 2.000000000000000000 ) ) ;
#8744 = ORIENTED_EDGE ( 'NONE', *, *, #12700, .F. ) ;
#8745 = VERTEX_POINT ( 'NONE', #12238 ) ;
#8746 = DIRECTION ( 'NONE',  ( 1.000000000000000000, -6.938893903907222067E-15, 0.000000000000000000 ) ) ;
#8747 = VERTEX_POINT ( 'NONE', #948 ) ;
#8748 = CARTESIAN_POINT ( 'NONE',  ( -13.37499999999998224, -20.24999999999998934, 4.166666666666636765 ) ) ;
#8749 = VECTOR ( 'NONE', #16715, 1000.000000000000000 ) ;
#8750 = EDGE_CURVE ( 'NONE', #18680, #932, #7443, .T. ) ;
#8751 = ORIENTED_EDGE ( 'NONE', *, *, #2628, .F. ) ;
#8752 = DIRECTION ( 'NONE',  ( 0.000000000000000000, 1.000000000000000000, 0.000000000000000000 ) ) ;
#8753 = LINE ( 'NONE', #18267, #15674 ) ;
#8754 = CARTESIAN_POINT ( 'NONE',  ( 0.000000000000000000, 9.000000000000001776, 0.000000000000000000 ) ) ;
#8755 = CARTESIAN_POINT ( 'NONE',  ( 1.337453470010121714, -9.114917468222230923, 2.372643865078341019 ) ) ;
#8756 = CARTESIAN_POINT ( 'NONE',  ( -6.152808582316794173, -21.22443879296942626, 5.229004561291660025 ) ) ;
#8757 = CARTESIAN_POINT ( 'NONE',  ( 13.87824226375436965, 4.413734319597230282, 6.694665752684481497 ) ) ;
#8758 = CARTESIAN_POINT ( 'NONE',  ( -15.11404127825609223, 4.999999999999999112, 1.000000000000000000 ) ) ;
#8759 = CARTESIAN_POINT ( 'NONE',  ( 5.878441417683177406, -23.74999999999999645, 3.449312527122335492 ) ) ;
#8760 = CARTESIAN_POINT ( 'NONE',  ( 15.50000000000001776, -17.49999999999999645, 4.000000000000000000 ) ) ;
#8761 = EDGE_CURVE ( 'NONE', #20538, #10727, #13591, .T. ) ;
#8762 = CARTESIAN_POINT ( 'NONE',  ( -5.222191417683177406, -21.02099543870834353, 3.964901035250761208 ) ) ;
#8763 = VECTOR ( 'NONE', #3493, 1000.000000000000000 ) ;
#8764 = CARTESIAN_POINT ( 'NONE',  ( -11.97219141768317918, -24.47900456129165292, 2.413778621189595963 ) ) ;
#8765 = ORIENTED_EDGE ( 'NONE', *, *, #5646, .F. ) ;
#8766 = CARTESIAN_POINT ( 'NONE',  ( 12.63958155142659834, -18.76363165295958524, 4.767928440007602298 ) ) ;
#8767 = CARTESIAN_POINT ( 'NONE',  ( -13.12424783836753228, 4.962015837561366993, 5.328858059679200565 ) ) ;
#8768 = ORIENTED_EDGE ( 'NONE', *, *, #19901, .F. ) ;
#8769 = LINE ( 'NONE', #13661, #12957 ) ;
#8770 = CARTESIAN_POINT ( 'NONE',  ( -22.85856191738413656, 0.000000000000000000, 1.000000000000000000 ) ) ;
#8771 = EDGE_LOOP ( 'NONE', ( #18467, #6191, #5176, #8637 ) ) ;
#8772 = ORIENTED_EDGE ( 'NONE', *, *, #13316, .F. ) ;
#8773 = ADVANCED_FACE ( 'NONE', ( #20306 ), #12448, .T. ) ;
#8774 = ADVANCED_FACE ( 'NONE', ( #4505 ), #5968, .T. ) ;
#8775 = EDGE_LOOP ( 'NONE', ( #15369, #791, #17864, #1580 ) ) ;
#8776 = DIRECTION ( 'NONE',  ( 0.000000000000000000, 0.000000000000000000, -1.000000000000000000 ) ) ;
#8777 = VECTOR ( 'NONE', #4315, 1000.000000000000000 ) ;
#8778 = CARTESIAN_POINT ( 'NONE',  ( -26.04469207716614676, 4.999999999999999112, 0.000000000000000000 ) ) ;
#8779 = ADVANCED_FACE ( 'NONE', ( #12343 ), #18737, .T. ) ;
#8780 = CARTESIAN_POINT ( 'NONE',  ( -2.195822829018478473, -9.226849102155203042, 1.651390144731336163 ) ) ;
#8781 = CARTESIAN_POINT ( 'NONE',  ( 0.000000000000000000, 4.999999999999999112, 1.000000000000000000 ) ) ;
#8782 = DIRECTION ( 'NONE',  ( -0.000000000000000000, 0.000000000000000000, 1.000000000000000000 ) ) ;
#8783 = CYLINDRICAL_SURFACE ( 'NONE', #18439, 2.999999999999999112 ) ;
#8784 = DIRECTION ( 'NONE',  ( 0.000000000000000000, 0.000000000000000000, 1.000000000000000000 ) ) ;
#8785 = CARTESIAN_POINT ( 'NONE',  ( 9.347191417683177406, -20.91377862118959285, 1.020995438708345082 ) ) ;
#8786 = CARTESIAN_POINT ( 'NONE',  ( -13.11514659413808737, 4.502403003978772134, 5.887634658581065494 ) ) ;
#8787 = EDGE_CURVE ( 'NONE', #13083, #13385, #14529, .T. ) ;
#8788 = CARTESIAN_POINT ( 'NONE',  ( -8.597191417683177406, -23.08622137881040359, 5.979004561291654696 ) ) ;
#8789 = ORIENTED_EDGE ( 'NONE', *, *, #10380, .F. ) ;
#8790 = CARTESIAN_POINT ( 'NONE',  ( 13.37155858231679417, -20.24999999999999289, 3.449312527122348371 ) ) ;
#8791 = CARTESIAN_POINT ( 'NONE',  ( 0.000000000000000000, 10.00000000000000000, 1.000000000000000000 ) ) ;
#8792 = CARTESIAN_POINT ( 'NONE',  ( -13.45671396861735403, -16.87344458480707843, 6.294109435864141844 ) ) ;
#8793 = VECTOR ( 'NONE', #4400, 1000.000000000000000 ) ;
#8794 = CARTESIAN_POINT ( 'NONE',  ( 5.027808582316795949, -22.97900456129165647, 3.964901035250747885 ) ) ;
#8795 = DIRECTION ( 'NONE',  ( 0.000000000000000000, 0.000000000000000000, -1.000000000000000000 ) ) ;
#8796 = VERTEX_POINT ( 'NONE', #8163 ) ;
#8797 = ORIENTED_EDGE ( 'NONE', *, *, #6286, .F. ) ;
#8798 = CARTESIAN_POINT ( 'NONE',  ( 13.85403523778986390, 3.941279508358651817, 5.991705257707216958 ) ) ;
#8799 = LINE ( 'NONE', #8898, #548 ) ;
#8800 = SURFACE_STYLE_USAGE ( .BOTH. , #5549 ) ;
#8801 = EDGE_LOOP ( 'NONE', ( #18257, #17548, #18733, #4569 ) ) ;
#8802 = CARTESIAN_POINT ( 'NONE',  ( -9.000000000000000000, -9.999999999999992895, 1.000000000000000000 ) ) ;
#8803 = DIRECTION ( 'NONE',  ( -1.000000000000000000, -2.312964634635731617E-15, 0.000000000000000000 ) ) ;
#8804 = LINE ( 'NONE', #18118, #1957 ) ;
#8805 = CARTESIAN_POINT ( 'NONE',  ( 13.58606361274418184, -9.591287556442823714, 5.700679699621803209 ) ) ;
#8806 = CARTESIAN_POINT ( 'NONE',  ( -2.061130159782011972, 9.000000000000001776, 1.000000000000000000 ) ) ;
#8807 = CARTESIAN_POINT ( 'NONE',  ( 3.336296098497695262, -9.936854405034125648, 2.776348673047012383 ) ) ;
#8808 = LINE ( 'NONE', #12037, #43 ) ;
#8809 = CARTESIAN_POINT ( 'NONE',  ( -12.62958809053144549, -19.26830142816300295, 4.757073430686623361 ) ) ;
#8810 = CARTESIAN_POINT ( 'NONE',  ( 0.000000000000000000, 4.999999999999999112, 0.000000000000000000 ) ) ;
#8811 = CARTESIAN_POINT ( 'NONE',  ( 11.30905858231679417, -23.27327832286945153, 2.298404588716537411 ) ) ;
#8812 = CARTESIAN_POINT ( 'NONE',  ( -13.43273460392801155, -18.08440250163749496, 6.268067769197452677 ) ) ;
#8813 = EDGE_CURVE ( 'NONE', #20051, #8358, #15994, .T. ) ;
#8814 = DIRECTION ( 'NONE',  ( 1.000000000000000000, 0.000000000000000000, -0.000000000000000000 ) ) ;
#8815 = CARTESIAN_POINT ( 'NONE',  ( 12.80905858231679417, -23.27327832286945153, 2.298404588716537411 ) ) ;
#8816 = CARTESIAN_POINT ( 'NONE',  ( 10.37844141768317741, -22.99999999999999645, 3.449312527122335048 ) ) ;
#8817 = CARTESIAN_POINT ( 'NONE',  ( -9.809058582316794173, -23.27327832286945153, 2.298404588716537411 ) ) ;
#8818 = VECTOR ( 'NONE', #2776, 1000.000000000000000 ) ;
#8819 = ORIENTED_EDGE ( 'NONE', *, *, #20608, .F. ) ;
#8820 = CARTESIAN_POINT ( 'NONE',  ( 12.66383876651304874, -19.03864229108970463, 6.262079579155994224 ) ) ;
#8821 = CARTESIAN_POINT ( 'NONE',  ( 12.62958809053144549, -19.26830142816300295, 4.757073430686623361 ) ) ;
#8822 = LINE ( 'NONE', #2430, #6685 ) ;
#8823 = ORIENTED_EDGE ( 'NONE', *, *, #1409, .F. ) ;
#8824 = UNCERTAINTY_MEASURE_WITH_UNIT (LENGTH_MEASURE( 1.000000000000000082E-05 ), #16287, 'distance_accuracy_value', 'NONE');
#8825 = ORIENTED_EDGE ( 'NONE', *, *, #17975, .T. ) ;
#8826 = LINE ( 'NONE', #2752, #15786 ) ;
#8827 = VECTOR ( 'NONE', #6027, 1000.000000000000000 ) ;
#8828 = CARTESIAN_POINT ( 'NONE',  ( 13.42791111847407848, 9.000000000000001776, 0.000000000000000000 ) ) ;
#8829 = CARTESIAN_POINT ( 'NONE',  ( 11.00000000000000000, -25.49999999999999645, 6.500000000000000000 ) ) ;
#8830 = LINE ( 'NONE', #18552, #2363 ) ;
#8831 = CARTESIAN_POINT ( 'NONE',  ( 1.548630333695928396, -9.114917468222230923, 2.372643865078341019 ) ) ;
#8832 = DIRECTION ( 'NONE',  ( -0.000000000000000000, -0.000000000000000000, -1.000000000000000000 ) ) ;
#8833 = DIRECTION ( 'NONE',  ( 0.000000000000000000, 1.000000000000000000, 0.000000000000000000 ) ) ;
#8834 = DIRECTION ( 'NONE',  ( 0.000000000000000000, 1.000000000000000000, -0.000000000000000000 ) ) ;
#8835 = CARTESIAN_POINT ( 'NONE',  ( -12.05905858231679595, -20.19639159124062999, 5.231925497173373074 ) ) ;
#8836 = CARTESIAN_POINT ( 'NONE',  ( -2.589709240944451096, -9.559844081062008669, 1.736909907557668165 ) ) ;
#8837 = ORIENTED_EDGE ( 'NONE', *, *, #13743, .F. ) ;
#8838 = CARTESIAN_POINT ( 'NONE',  ( -13.37908441539295801, -19.29373702265862889, 4.740102594697787275 ) ) ;
#8839 = CARTESIAN_POINT ( 'NONE',  ( -9.527808582316792396, -23.72900456129165647, 4.275561207030568411 ) ) ;
#8840 = ADVANCED_FACE ( 'NONE', ( #17669 ), #14423, .T. ) ;
#8841 = CARTESIAN_POINT ( 'NONE',  ( 7.840308582316795949, -22.98484643305508612, 6.020995438708344416 ) ) ;
#8842 = CARTESIAN_POINT ( 'NONE',  ( -10.00344141768317741, -22.05068747287766229, 4.499999999999999112 ) ) ;
#8843 = VERTEX_POINT ( 'NONE', #9514 ) ;
#8844 = CARTESIAN_POINT ( 'NONE',  ( 13.37499999999998579, -20.24999999999999289, 3.666666666666653640 ) ) ;
#8845 = DIRECTION ( 'NONE',  ( -1.000000000000000000, 0.000000000000000000, 0.000000000000000000 ) ) ;
#8846 = ORIENTED_EDGE ( 'NONE', *, *, #20468, .T. ) ;
#8847 = ORIENTED_EDGE ( 'NONE', *, *, #8029, .T. ) ;
#8848 = DIRECTION ( 'NONE',  ( -1.000000000000000000, 0.000000000000000000, 0.000000000000000000 ) ) ;
#8849 = ORIENTED_EDGE ( 'NONE', *, *, #1690, .T. ) ;
#8850 = CARTESIAN_POINT ( 'NONE',  ( -13.37515323800563039, -20.24226148071262799, 4.627790572011877934 ) ) ;
#8851 = EDGE_CURVE ( 'NONE', #5957, #15361, #16107, .T. ) ;
#8852 = ORIENTED_EDGE ( 'NONE', *, *, #6500, .F. ) ;
#8853 = DIRECTION ( 'NONE',  ( 0.000000000000000000, 1.000000000000000000, 0.000000000000000000 ) ) ;
#8854 = DIRECTION ( 'NONE',  ( 0.000000000000000000, 0.000000000000000000, -1.000000000000000000 ) ) ;
#8855 = CARTESIAN_POINT ( 'NONE',  ( 13.92791111847407848, 9.000000000000001776, 1.000000000000000000 ) ) ;
#8856 = CARTESIAN_POINT ( 'NONE',  ( 3.317048600639548095, -9.800042196285016161, 2.741212564741740465 ) ) ;
#8857 = PLANE ( 'NONE',  #8255 ) ;
#8858 = VECTOR ( 'NONE', #2812, 1000.000000000000000 ) ;
#8859 = CARTESIAN_POINT ( 'NONE',  ( 13.90439735423812273, 5.734566389025032684, 3.666666666666500873 ) ) ;
#8860 = DIRECTION ( 'NONE',  ( -1.000000000000000000, -0.000000000000000000, -0.000000000000000000 ) ) ;
#8861 = CARTESIAN_POINT ( 'NONE',  ( 10.47219141768317741, -22.97900456129165292, 3.035098964749240125 ) ) ;
#8862 = PLANE ( 'NONE',  #15225 ) ;
#8863 = CARTESIAN_POINT ( 'NONE',  ( -7.565941417683177406, -22.67126532539353789, 2.757051763020445634 ) ) ;
#8864 = EDGE_CURVE ( 'NONE', #3392, #20119, #19255, .T. ) ;
#8865 = CARTESIAN_POINT ( 'NONE',  ( -8.034691417683175629, -19.47900456129164581, 2.515153566944927199 ) ) ;
#8866 = EDGE_LOOP ( 'NONE', ( #9918, #12951, #13641, #5962 ) ) ;
#8867 = CARTESIAN_POINT ( 'NONE',  ( 13.12526104302547836, 5.013182672784613381, 5.066812735559260261 ) ) ;
#8868 = CARTESIAN_POINT ( 'NONE',  ( -13.12529397354238192, 5.014845663890295846, 3.666666666666500873 ) ) ;
#8869 = ORIENTED_EDGE ( 'NONE', *, *, #4630, .T. ) ;
#8870 = LINE ( 'NONE', #15240, #1601 ) ;
#8871 = CARTESIAN_POINT ( 'NONE',  ( 13.50000000000000178, 7.806255641895631925E-15, 2.000000000000000000 ) ) ;
#8872 = ORIENTED_EDGE ( 'NONE', *, *, #17986, .T. ) ;
#8873 = ORIENTED_EDGE ( 'NONE', *, *, #5909, .T. ) ;
#8874 = VECTOR ( 'NONE', #3738, 1000.000000000000000 ) ;
#8875 = ORIENTED_EDGE ( 'NONE', *, *, #13780, .F. ) ;
#8876 = EDGE_CURVE ( 'NONE', #20251, #3865, #12643, .T. ) ;
#8877 = CARTESIAN_POINT ( 'NONE',  ( 0.000000000000000000, 4.999999999999999112, 1.000000000000000000 ) ) ;
#8878 = CARTESIAN_POINT ( 'NONE',  ( -14.49999999999998579, -18.49999999999999645, 4.000000000000000000 ) ) ;
#8879 = CARTESIAN_POINT ( 'NONE',  ( -2.682825141213236009, -9.727160171598653093, 1.779880022082258373 ) ) ;
#8880 = DIRECTION ( 'NONE',  ( -0.000000000000000000, -0.000000000000000000, -1.000000000000000000 ) ) ;
#8881 = DIRECTION ( 'NONE',  ( 1.000000000000000000, 0.000000000000000000, 0.000000000000000000 ) ) ;
#8882 = LINE ( 'NONE', #1037, #337 ) ;
#8883 = CARTESIAN_POINT ( 'NONE',  ( 6.059058582316795949, -20.19639159124062999, 5.231925497173373074 ) ) ;
#8884 = CARTESIAN_POINT ( 'NONE',  ( -12.64511805349267526, -19.23403829861753422, 5.507852591554869726 ) ) ;
#8885 = CARTESIAN_POINT ( 'NONE',  ( -6.722191417683176518, -19.52099543870834353, 4.586221378810406257 ) ) ;
#8886 = EDGE_CURVE ( 'NONE', #3209, #15372, #12953, .T. ) ;
#8887 = ORIENTED_EDGE ( 'NONE', *, *, #4755, .T. ) ;
#8888 = ADVANCED_FACE ( 'NONE', ( #5013 ), #12853, .T. ) ;
#8889 = CARTESIAN_POINT ( 'NONE',  ( -4.000000000000000000, -12.50000000000000000, 3.464723819589916154 ) ) ;
#8890 = DIRECTION ( 'NONE',  ( 1.000000000000000000, 3.469446951953619119E-16, -0.000000000000000000 ) ) ;
#8891 = CARTESIAN_POINT ( 'NONE',  ( -13.41834698511420676, -18.81097725173551893, 6.252442769197418926 ) ) ;
#8892 = VECTOR ( 'NONE', #15333, 1000.000000000000000 ) ;
#8893 = CARTESIAN_POINT ( 'NONE',  ( 12.80905858231679417, -23.27327832286945153, 2.298404588716537411 ) ) ;
#8894 = PLANE ( 'NONE',  #18008 ) ;
#8895 = ORIENTED_EDGE ( 'NONE', *, *, #16297, .T. ) ;
#8896 = ORIENTED_EDGE ( 'NONE', *, *, #1907, .F. ) ;
#8897 = CARTESIAN_POINT ( 'NONE',  ( 13.84863765609603625, 3.668701632846259830, 5.985835949623216301 ) ) ;
#8898 = CARTESIAN_POINT ( 'NONE',  ( -9.305650798910056309, 0.000000000000000000, 0.000000000000000000 ) ) ;
#8899 = ORIENTED_EDGE ( 'NONE', *, *, #10162, .T. ) ;
#8900 = DIRECTION ( 'NONE',  ( 0.000000000000000000, 0.000000000000000000, 1.000000000000000000 ) ) ;
#8901 = LINE ( 'NONE', #3878, #8375 ) ;
#8902 = EDGE_CURVE ( 'NONE', #95, #15413, #20619, .T. ) ;
#8903 = DIRECTION ( 'NONE',  ( 1.000000000000000000, -0.000000000000000000, 0.000000000000000000 ) ) ;
#8904 = CARTESIAN_POINT ( 'NONE',  ( 13.87470602645761986, 4.985154336109792972, 4.583333333333296622 ) ) ;
#8905 = DIRECTION ( 'NONE',  ( 1.000000000000000000, 0.000000000000000000, -0.000000000000000000 ) ) ;
#8906 = CARTESIAN_POINT ( 'NONE',  ( 1.906542528716098417, -8.376716462152538512, 1.625674082428238298 ) ) ;
#8907 = CARTESIAN_POINT ( 'NONE',  ( -0.000000000000000000, 11.64110105645932691, 0.000000000000000000 ) ) ;
#8908 = CARTESIAN_POINT ( 'NONE',  ( -13.09556065010287362, 4.263312830196960057, 5.034075356110313315 ) ) ;
#8909 = DIRECTION ( 'NONE',  ( -1.156482317317871331E-15, 1.000000000000000000, -0.000000000000000000 ) ) ;
#8910 = CARTESIAN_POINT ( 'NONE',  ( -13.86436316834274329, 3.712840001305938831, 6.736817769197426031 ) ) ;
#8911 = EDGE_CURVE ( 'NONE', #13563, #2750, #2382, .T. ) ;
#8912 = CARTESIAN_POINT ( 'NONE',  ( -13.50000000000000178, 0.000000000000000000, 1.000000000000000000 ) ) ;
#8913 = CARTESIAN_POINT ( 'NONE',  ( 12.43405858231679417, -23.20159541128345992, 4.773278322869455970 ) ) ;
#8914 = CARTESIAN_POINT ( 'NONE',  ( 4.003441417683176518, -22.05068747287765873, 5.250000000000000888 ) ) ;
#8915 = CARTESIAN_POINT ( 'NONE',  ( -12.43405858231679417, -23.20159541128345992, 4.773278322869455970 ) ) ;
#8916 = ORIENTED_EDGE ( 'NONE', *, *, #19803, .T. ) ;
#8917 = CARTESIAN_POINT ( 'NONE',  ( 13.01365964058540037, 0.1273118495903458325, 5.174178440007729307 ) ) ;
#8918 = LINE ( 'NONE', #18544, #20386 ) ;
#8919 = VERTEX_POINT ( 'NONE', #3547 ) ;
#8920 = VERTEX_POINT ( 'NONE', #9925 ) ;
#8921 = FACE_OUTER_BOUND ( 'NONE', #4878, .T. ) ;
#8922 = EDGE_CURVE ( 'NONE', #17043, #11975, #14933, .T. ) ;
#8923 = CARTESIAN_POINT ( 'NONE',  ( -12.79798428357658047, -11.51429367935891790, 5.673858176248284479 ) ) ;
#8924 = CARTESIAN_POINT ( 'NONE',  ( -3.162271481458107658, -13.95306990448253437, 3.615178062515473911 ) ) ;
#8925 = CARTESIAN_POINT ( 'NONE',  ( -13.84264281492353987, 3.365962153638767607, 5.979325532956542233 ) ) ;
#8926 = DIRECTION ( 'NONE',  ( -0.000000000000000000, -0.000000000000000000, -1.000000000000000000 ) ) ;
#8927 = CARTESIAN_POINT ( 'NONE',  ( 2.436080212393455735, -9.483920418190111334, 2.467411194204634839 ) ) ;
#8928 = FACE_OUTER_BOUND ( 'NONE', #15368, .T. ) ;
#8929 = CARTESIAN_POINT ( 'NONE',  ( -3.997260319564023501, 0.000000000000000000, 0.000000000000000000 ) ) ;
#8930 = CARTESIAN_POINT ( 'NONE',  ( -0.5631383031621635116, -9.114917468222230923, 2.372643865078341019 ) ) ;
#8931 = CARTESIAN_POINT ( 'NONE',  ( -8.965308582316795949, -19.47900456129164937, 4.484846433055089676 ) ) ;
#8932 = CARTESIAN_POINT ( 'NONE',  ( -3.232228556578340850, -13.29361487011126464, 2.695816835751057461 ) ) ;
#8933 = ORIENTED_EDGE ( 'NONE', *, *, #15625, .F. ) ;
#8934 = CARTESIAN_POINT ( 'NONE',  ( -13.09560264576187905, 4.265433610975056133, 4.333333333333380999 ) ) ;
#8935 = DIRECTION ( 'NONE',  ( -0.000000000000000000, 0.000000000000000000, -1.000000000000000000 ) ) ;
#8936 = CARTESIAN_POINT ( 'NONE',  ( 6.434058582316796837, -23.73192549717337130, 5.303608408759367343 ) ) ;
#8937 = CARTESIAN_POINT ( 'NONE',  ( -8.784691417683177406, -23.02099543870834353, 3.863526089495429972 ) ) ;
#8938 = ORIENTED_EDGE ( 'NONE', *, *, #2318, .F. ) ;
#8939 = CARTESIAN_POINT ( 'NONE',  ( 13.37499999999998224, -20.25000000000006395, 4.416666666666681174 ) ) ;
#8940 = DIRECTION ( 'NONE',  ( 0.000000000000000000, -1.000000000000000000, 0.000000000000000000 ) ) ;
#8941 = ORIENTED_EDGE ( 'NONE', *, *, #10313, .T. ) ;
#8942 = VERTEX_POINT ( 'NONE', #612 ) ;
#8943 = CARTESIAN_POINT ( 'NONE',  ( -13.81494360078803396, 10.00000000000000000, 0.000000000000000000 ) ) ;
#8944 = VERTEX_POINT ( 'NONE', #8363 ) ;
#8945 = CARTESIAN_POINT ( 'NONE',  ( -13.86693669322925260, 4.592803008081209448, 5.801483467520450077 ) ) ;
#8946 = ORIENTED_EDGE ( 'NONE', *, *, #6940, .F. ) ;
#8947 = DIRECTION ( 'NONE',  ( -0.000000000000000000, 0.000000000000000000, -1.000000000000000000 ) ) ;
#8948 = DIRECTION ( 'NONE',  ( 1.000000000000000000, -0.000000000000000000, 0.000000000000000000 ) ) ;
#8949 = EDGE_CURVE ( 'NONE', #11770, #1149, #11595, .T. ) ;
#8950 = CARTESIAN_POINT ( 'NONE',  ( 0.000000000000000000, 9.000000000000001776, 0.000000000000000000 ) ) ;
#8951 = CARTESIAN_POINT ( 'NONE',  ( 1.548630333695928396, -9.114917468222230923, 2.372643865078341019 ) ) ;
#8952 = LINE ( 'NONE', #10738, #3846 ) ;
#8953 = CARTESIAN_POINT ( 'NONE',  ( 13.88045627189955233, 4.525541730927888473, 6.662882075361062029 ) ) ;
#8954 = PLANE ( 'NONE',  #9307 ) ;
#8955 = CARTESIAN_POINT ( 'NONE',  ( 13.42791111847407848, 4.999999999999999112, 1.000000000000000000 ) ) ;
#8956 = CARTESIAN_POINT ( 'NONE',  ( 13.12529397354238192, 5.014845663890295846, 4.166666666666765551 ) ) ;
#8957 = CARTESIAN_POINT ( 'NONE',  ( 12.25344141768317741, -21.94931252712233061, 2.499999999999999112 ) ) ;
#8958 = DIRECTION ( 'NONE',  ( 1.734723475976807094E-15, 1.000000000000000000, 0.000000000000000000 ) ) ;
#8959 = CARTESIAN_POINT ( 'NONE',  ( -5.034691417683177406, -20.97900456129164581, 3.136473910504570917 ) ) ;
#8960 = CARTESIAN_POINT ( 'NONE',  ( -11.22219141768317741, -19.52099543870834353, 4.586221378810406257 ) ) ;
#8961 = VECTOR ( 'NONE', #17760, 1000.000000000000000 ) ;
#8962 = ORIENTED_EDGE ( 'NONE', *, *, #4983, .T. ) ;
#8963 = CARTESIAN_POINT ( 'NONE',  ( 12.66835678905406049, -17.31048215276408797, 4.799178440007564994 ) ) ;
#8964 = CARTESIAN_POINT ( 'NONE',  ( -13.09293046926041626, 3.380488697651010011, 5.994170676248444352 ) ) ;
#8965 = ORIENTED_EDGE ( 'NONE', *, *, #9182, .T. ) ;
#8966 = VECTOR ( 'NONE', #18510, 1000.000000000000000 ) ;
#8967 = PLANE ( 'NONE',  #5270 ) ;
#8968 = FACE_OUTER_BOUND ( 'NONE', #6556, .T. ) ;
#8969 = EDGE_LOOP ( 'NONE', ( #798, #1976, #17500, #1795 ) ) ;
#8970 = CARTESIAN_POINT ( 'NONE',  ( 2.436080212393455735, -9.483920418190111334, 2.467411194204634839 ) ) ;
#8971 = ORIENTED_EDGE ( 'NONE', *, *, #14251, .T. ) ;
#8972 = AXIS2_PLACEMENT_3D ( 'NONE', #4551, #14367, #52 ) ;
#8973 = VERTEX_POINT ( 'NONE', #19873 ) ;
#8974 = DIRECTION ( 'NONE',  ( 0.000000000000000000, 0.000000000000000000, 1.000000000000000000 ) ) ;
#8975 = LINE ( 'NONE', #5844, #625 ) ;
#8976 = EDGE_CURVE ( 'NONE', #14732, #3716, #5630, .T. ) ;
#8977 = VECTOR ( 'NONE', #12811, 1000.000000000000000 ) ;
#8978 = CARTESIAN_POINT ( 'NONE',  ( -2.050137595624097031, -10.15260257655714504, 1.696527147986202522 ) ) ;
#8979 = CARTESIAN_POINT ( 'NONE',  ( -7.869520639128047002, 9.000000000000001776, 0.000000000000000000 ) ) ;
#8980 = LINE ( 'NONE', #7422, #5112 ) ;
#8981 = VECTOR ( 'NONE', #12609, 1000.000000000000000 ) ;
#8982 = LINE ( 'NONE', #4269, #7360 ) ;
#8983 = EDGE_CURVE ( 'NONE', #1283, #4081, #16820, .T. ) ;
#8984 = EDGE_CURVE ( 'NONE', #8181, #16994, #7207, .T. ) ;
#8985 = CARTESIAN_POINT ( 'NONE',  ( 5.309058582316795949, -23.80360840875935935, 1.768074502826626260 ) ) ;
#8986 = CARTESIAN_POINT ( 'NONE',  ( -12.62745083560477966, -20.12623280195927933, 5.001038150054709419 ) ) ;
#8987 = CARTESIAN_POINT ( 'NONE',  ( -4.565941417683176518, -23.73192549717336064, 1.696391591240623331 ) ) ;
#8988 = EDGE_LOOP ( 'NONE', ( #12112, #1921, #4176, #18056, #5320 ) ) ;
#8989 = CARTESIAN_POINT ( 'NONE',  ( -0.1250000000000035805, 4.999999999999999112, 1.000000000000000000 ) ) ;
#8990 = AXIS2_PLACEMENT_3D ( 'NONE', #9590, #20285, #12524 ) ;
#8991 = LINE ( 'NONE', #10662, #6421 ) ;
#8992 = CARTESIAN_POINT ( 'NONE',  ( -13.50467269799730374, -14.45152875114793467, 6.346192769197517514 ) ) ;
#8993 = VECTOR ( 'NONE', #14683, 1000.000000000000000 ) ;
#8994 = CARTESIAN_POINT ( 'NONE',  ( 12.52780858231679595, -23.72900456129165647, 4.275561207030568411 ) ) ;
#8995 = FACE_OUTER_BOUND ( 'NONE', #13626, .T. ) ;
#8996 = VECTOR ( 'NONE', #7221, 1000.000000000000000 ) ;
#8997 = EDGE_LOOP ( 'NONE', ( #20070, #13639, #2196, #2103 ) ) ;
#8998 = EDGE_LOOP ( 'NONE', ( #9241, #13051, #19723, #13468 ) ) ;
#8999 = CARTESIAN_POINT ( 'NONE',  ( 13.56222317325195093, -11.54522975075300728, 6.408692769197242178 ) ) ;
#9000 = AXIS2_PLACEMENT_3D ( 'NONE', #16892, #20256, #15529 ) ;
#9001 = CARTESIAN_POINT ( 'NONE',  ( 5.381197846483058989, -6.000000000000000000, 2.000000000000000000 ) ) ;
#9002 = ORIENTED_EDGE ( 'NONE', *, *, #16904, .T. ) ;
#9003 = DIRECTION ( 'NONE',  ( 0.000000000000000000, 1.000000000000000000, -0.000000000000000000 ) ) ;
#9004 = VERTEX_POINT ( 'NONE', #13781 ) ;
#9005 = CARTESIAN_POINT ( 'NONE',  ( -13.18405858231679417, -20.79840458871652942, 2.226721677130544030 ) ) ;
#9006 = DIRECTION ( 'NONE',  ( 4.625929269271486900E-15, 1.000000000000000000, 0.000000000000000000 ) ) ;
#9007 = ADVANCED_FACE ( 'NONE', ( #15148 ), #6053, .F. ) ;
#9008 = LINE ( 'NONE', #7544, #1842 ) ;
#9009 = AXIS2_PLACEMENT_3D ( 'NONE', #20257, #5500, #2360 ) ;
#9010 = CARTESIAN_POINT ( 'NONE',  ( 2.682825141213236009, -9.727160171598653093, 1.779880022082258373 ) ) ;
#9011 = CIRCLE ( 'NONE', #4336, 0.3749999999999998890 ) ;
#9012 = LINE ( 'NONE', #18323, #6721 ) ;
#9013 = CARTESIAN_POINT ( 'NONE',  ( -13.09560264576187905, 4.265433610975056133, 3.666666666666500873 ) ) ;
#9014 = CARTESIAN_POINT ( 'NONE',  ( 11.21530858231679417, -23.77099543870833998, 2.825813738724734847 ) ) ;
#9015 = CARTESIAN_POINT ( 'NONE',  ( -13.50467269799730374, -14.45152875114793467, 6.346192769197517514 ) ) ;
#9016 = VECTOR ( 'NONE', #19519, 1000.000000000000114 ) ;
#9017 = CARTESIAN_POINT ( 'NONE',  ( 6.063547257480584207, 16.00000000000000000, 1.000000000000000000 ) ) ;
#9018 = CARTESIAN_POINT ( 'NONE',  ( 5.871558582316795949, -20.99999999999999645, 3.449312527122348371 ) ) ;
#9019 = CARTESIAN_POINT ( 'NONE',  ( 10.28469141768317741, -23.02099543870834353, 3.863526089495429972 ) ) ;
#9020 = CARTESIAN_POINT ( 'NONE',  ( -11.96530858231679595, -20.22900456129164937, 4.174186261275266929 ) ) ;
#9021 = VERTEX_POINT ( 'NONE', #7614 ) ;
#9022 = CARTESIAN_POINT ( 'NONE',  ( 13.37908441539295801, -19.29373702265862889, 4.740102594697787275 ) ) ;
#9023 = DIRECTION ( 'NONE',  ( 0.000000000000000000, 0.000000000000000000, 1.000000000000000000 ) ) ;
#9024 = ORIENTED_EDGE ( 'NONE', *, *, #13835, .F. ) ;
#9025 = MECHANICAL_DESIGN_GEOMETRIC_PRESENTATION_REPRESENTATION (  '', ( #20054 ), #6697 ) ;
#9026 = VERTEX_POINT ( 'NONE', #8778 ) ;
#9027 = LINE ( 'NONE', #7560, #18472 ) ;
#9028 = VECTOR ( 'NONE', #847, 1000.000000000000000 ) ;
#9029 = CARTESIAN_POINT ( 'NONE',  ( -26.04469207716615031, 9.000000000000001776, 1.000000000000000000 ) ) ;
#9030 = EDGE_CURVE ( 'NONE', #19766, #9549, #2387, .T. ) ;
#9031 = ADVANCED_FACE ( 'NONE', ( #10548 ), #20283, .T. ) ;
#9032 = CARTESIAN_POINT ( 'NONE',  ( -2.731427961995660958, -10.89409100229510052, 2.829571171190552015 ) ) ;
#9033 = CARTESIAN_POINT ( 'NONE',  ( -13.87215786865436762, 4.856472367046606564, 5.506273593909547515 ) ) ;
#9034 = CARTESIAN_POINT ( 'NONE',  ( 14.99999999999999645, 3.000000000000003553, 2.000000000000000000 ) ) ;
#9035 = FACE_OUTER_BOUND ( 'NONE', #3773, .T. ) ;
#9036 = CARTESIAN_POINT ( 'NONE',  ( -0.1250000000000035805, 9.000000000000000000, 0.000000000000000000 ) ) ;
#9037 = DIRECTION ( 'NONE',  ( -1.000000000000000000, 0.000000000000000000, 0.000000000000000000 ) ) ;
#9038 = CARTESIAN_POINT ( 'NONE',  ( -14.49999999999998579, -18.49999999999999645, 4.000000000000000000 ) ) ;
#9039 = CARTESIAN_POINT ( 'NONE',  ( -11.68405858231679595, -20.26807450282662160, 1.696391591240633101 ) ) ;
#9040 = CARTESIAN_POINT ( 'NONE',  ( -3.002445346198714837, -11.66215945560911749, 2.276826493710632171 ) ) ;
#9041 = VERTEX_POINT ( 'NONE', #16711 ) ;
#9042 = CARTESIAN_POINT ( 'NONE',  ( -13.37515323800563039, -20.24226148071262799, 4.627790572011877934 ) ) ;
#9043 = PRESENTATION_LAYER_ASSIGNMENT (  '', '', ( #1680 ) ) ;
#9044 = FACE_OUTER_BOUND ( 'NONE', #2026, .T. ) ;
#9045 = EDGE_CURVE ( 'NONE', #5093, #4793, #2808, .T. ) ;
#9046 = VECTOR ( 'NONE', #8803, 1000.000000000000000 ) ;
#9047 = CARTESIAN_POINT ( 'NONE',  ( 6.340308582316796837, -22.98484643305508612, 6.020995438708344416 ) ) ;
#9048 = CARTESIAN_POINT ( 'NONE',  ( -7.847191417683175629, -21.53509896474923835, 2.520995438708346192 ) ) ;
#9049 = VERTEX_POINT ( 'NONE', #18290 ) ;
#9050 = CARTESIAN_POINT ( 'NONE',  ( 13.39170256340046095, -19.40652054827866380, 5.481861153867630065 ) ) ;
#9051 = CARTESIAN_POINT ( 'NONE',  ( 14.50000000000000000, -23.00000000000001421, 4.000000000000000000 ) ) ;
#9052 = ORIENTED_EDGE ( 'NONE', *, *, #16608, .F. ) ;
#9053 = ORIENTED_EDGE ( 'NONE', *, *, #8607, .T. ) ;
#9054 = FACE_OUTER_BOUND ( 'NONE', #19378, .T. ) ;
#9055 = EDGE_LOOP ( 'NONE', ( #3803, #9306, #9793, #3091 ) ) ;
#9056 = CARTESIAN_POINT ( 'NONE',  ( -13.85788212999909419, 4.135547564954428879, 5.982801014393342776 ) ) ;
#9057 = DIRECTION ( 'NONE',  ( 1.000000000000000000, 0.000000000000000000, 0.000000000000000000 ) ) ;
#9058 = AXIS2_PLACEMENT_3D ( 'NONE', #8268, #14748, #212 ) ;
#9059 = VERTEX_POINT ( 'NONE', #7518 ) ;
#9060 = PLANE ( 'NONE',  #13285 ) ;
#9061 = CARTESIAN_POINT ( 'NONE',  ( 11.99999999999999822, -17.50000000000000000, 4.000000000000000000 ) ) ;
#9062 = VECTOR ( 'NONE', #11647, 1000.000000000000000 ) ;
#9063 = VECTOR ( 'NONE', #5046, 1000.000000000000000 ) ;
#9064 = LINE ( 'NONE', #7697, #2305 ) ;
#9065 = CARTESIAN_POINT ( 'NONE',  ( 3.385922596301560894, -9.481287983549590237, 1.909350115156127403 ) ) ;
#9066 = DIRECTION ( 'NONE',  ( 0.000000000000000000, 1.000000000000000000, 0.000000000000000000 ) ) ;
#9067 = CARTESIAN_POINT ( 'NONE',  ( 19.73630159782011617, 4.999999999999999112, 0.000000000000000000 ) ) ;
#9068 = LINE ( 'NONE', #8955, #8048 ) ;
#9069 = LINE ( 'NONE', #13964, #19042 ) ;
#9070 = CARTESIAN_POINT ( 'NONE',  ( 10.84719141768317741, -21.53509896474923835, 2.520995438708346192 ) ) ;
#9071 = CARTESIAN_POINT ( 'NONE',  ( -12.64131715375063258, -19.42598373559290792, 5.491151580003103660 ) ) ;
#9072 = CARTESIAN_POINT ( 'NONE',  ( -12.99655858231679595, -22.05068747287764452, 2.499999999999999112 ) ) ;
#9073 = EDGE_CURVE ( 'NONE', #20665, #2900, #823, .T. ) ;
#9074 = CARTESIAN_POINT ( 'NONE',  ( -11.87844141768317741, -24.50000000000000000, 3.449312527122335048 ) ) ;
#9075 = ORIENTED_EDGE ( 'NONE', *, *, #12942, .F. ) ;
#9076 = CARTESIAN_POINT ( 'NONE',  ( 12.62503976493681535, -19.49799187068907713, 4.533161381885315144 ) ) ;
#9077 = CARTESIAN_POINT ( 'NONE',  ( -12.66369984131459070, -18.29565801360988075, 5.528024842915327142 ) ) ;
#9078 = VERTEX_POINT ( 'NONE', #8878 ) ;
#9079 = AXIS2_PLACEMENT_3D ( 'NONE', #11220, #17596, #11122 ) ;
#9080 = LINE ( 'NONE', #16592, #273 ) ;
#9081 = CARTESIAN_POINT ( 'NONE',  ( 0.000000000000000000, 4.999999999999999112, 1.000000000000000000 ) ) ;
#9082 = VERTEX_POINT ( 'NONE', #13981 ) ;
#9083 = CARTESIAN_POINT ( 'NONE',  ( 1.957016269584227031, -9.152392576945766578, 2.382268221639079364 ) ) ;
#9084 = ORIENTED_EDGE ( 'NONE', *, *, #11779, .T. ) ;
#9085 = PLANE ( 'NONE',  #11000 ) ;
#9086 = DIRECTION ( 'NONE',  ( -0.4999999999999950040, 0.8660254037844415942, 0.000000000000000000 ) ) ;
#9087 = CARTESIAN_POINT ( 'NONE',  ( -2.327620134574780231, -13.27885108724501251, 3.249410218619480872 ) ) ;
#9088 = DIRECTION ( 'NONE',  ( 0.000000000000000000, 0.000000000000000000, 1.000000000000000000 ) ) ;
#9089 = DIRECTION ( 'NONE',  ( 1.000000000000000000, 0.000000000000000000, 0.000000000000000000 ) ) ;
#9090 = DIRECTION ( 'NONE',  ( 0.000000000000000000, -1.000000000000000000, 0.000000000000000000 ) ) ;
#9091 = CARTESIAN_POINT ( 'NONE',  ( 5.027808582316795949, -24.47900456129166358, 4.586221378810390270 ) ) ;
#9092 = CARTESIAN_POINT ( 'NONE',  ( -13.09532840572934376, 3.501584489333809724, 5.996774842915142401 ) ) ;
#9093 = CARTESIAN_POINT ( 'NONE',  ( -12.44094141768317741, -20.72672167713052715, 2.298404588716546293 ) ) ;
#9094 = ORIENTED_EDGE ( 'NONE', *, *, #1472, .T. ) ;
#9095 = CARTESIAN_POINT ( 'NONE',  ( 11.21530858231679417, -23.77099543870833998, 2.825813738724734847 ) ) ;
#9096 = CYLINDRICAL_SURFACE ( 'NONE', #2070, 10.00000000000000000 ) ;
#9097 = CARTESIAN_POINT ( 'NONE',  ( -13.77324158252158171, -0.8888000826463379189, 6.637859435864801760 ) ) ;
#9098 = EDGE_CURVE ( 'NONE', #12874, #16270, #20390, .T. ) ;
#9099 = CARTESIAN_POINT ( 'NONE',  ( 11.87155858231679417, -20.24999999999999289, 3.449312527122348371 ) ) ;
#9100 = DIRECTION ( 'NONE',  ( 0.000000000000000000, 1.000000000000000000, -0.000000000000000000 ) ) ;
#9101 = ORIENTED_EDGE ( 'NONE', *, *, #2777, .T. ) ;
#9102 = EDGE_LOOP ( 'NONE', ( #1463, #3206 ) ) ;
#9103 = CARTESIAN_POINT ( 'NONE',  ( 13.37499999999998224, -21.00000000000006395, 4.416666666666682062 ) ) ;
#9104 = CARTESIAN_POINT ( 'NONE',  ( 17.30017143803810242, 9.000000000000001776, 1.000000000000000000 ) ) ;
#9105 = EDGE_LOOP ( 'NONE', ( #9380, #6730, #16938, #3258, #19510, #8414, #8444, #19699, #7796, #8205 ) ) ;
#9106 = VECTOR ( 'NONE', #17100, 1000.000000000000000 ) ;
#9107 = DIRECTION ( 'NONE',  ( -0.000000000000000000, -0.000000000000000000, -1.000000000000000000 ) ) ;
#9108 = EDGE_CURVE ( 'NONE', #13797, #14476, #12314, .T. ) ;
#9109 = EDGE_CURVE ( 'NONE', #4154, #12358, #15246, .T. ) ;
#9110 = ORIENTED_EDGE ( 'NONE', *, *, #13948, .F. ) ;
#9111 = CARTESIAN_POINT ( 'NONE',  ( -10.27780858231679417, -20.27099543870833642, 2.724438792969431589 ) ) ;
#9112 = CARTESIAN_POINT ( 'NONE',  ( 13.87470623115321899, 4.985164673244912414, 4.958488177337359026 ) ) ;
#9113 = PLANE ( 'NONE',  #15822 ) ;
#9114 = CARTESIAN_POINT ( 'NONE',  ( 2.195822829018478473, -9.226849102155203042, 1.651390144731336163 ) ) ;
#9115 = DIRECTION ( 'NONE',  ( 0.000000000000000000, 0.000000000000000000, 1.000000000000000000 ) ) ;
#9116 = CARTESIAN_POINT ( 'NONE',  ( -13.09560269887985307, 4.265436293439658577, 4.973800642626965640 ) ) ;
#9117 = FACE_OUTER_BOUND ( 'NONE', #11323, .T. ) ;
#9118 = CARTESIAN_POINT ( 'NONE',  ( -13.37607268932110038, -20.94582918928111681, 4.945564004704174010 ) ) ;
#9119 = VECTOR ( 'NONE', #13304, 1000.000000000000000 ) ;
#9120 = DIRECTION ( 'NONE',  ( 0.000000000000000000, 0.000000000000000000, -1.000000000000000000 ) ) ;
#9121 = CARTESIAN_POINT ( 'NONE',  ( 9.715308582316794173, -23.77099543870833998, 2.825813738724734847 ) ) ;
#9122 = EDGE_CURVE ( 'NONE', #5545, #1638, #13567, .T. ) ;
#9123 = CARTESIAN_POINT ( 'NONE',  ( 3.944195004867016241, -21.61378581760806838, 5.207602947182413899 ) ) ;
#9124 = CARTESIAN_POINT ( 'NONE',  ( -10.65969141768317918, -22.67418626127524917, 1.729004561291651587 ) ) ;
#9125 = ORIENTED_EDGE ( 'NONE', *, *, #5592, .F. ) ;
#9126 = CARTESIAN_POINT ( 'NONE',  ( 13.09560264576187905, 4.265433610975056133, 3.666666666666500873 ) ) ;
#9127 = DIRECTION ( 'NONE',  ( 1.000000000000000000, 2.312964634635730039E-15, 0.000000000000000000 ) ) ;
#9128 = ORIENTED_EDGE ( 'NONE', *, *, #10521, .T. ) ;
#9129 = ORIENTED_EDGE ( 'NONE', *, *, #17929, .T. ) ;
#9130 = CARTESIAN_POINT ( 'NONE',  ( 20.49999999999998224, -21.99999999999999645, 11.00000000000000178 ) ) ;
#9131 = VECTOR ( 'NONE', #13903, 1000.000000000000000 ) ;
#9132 = CARTESIAN_POINT ( 'NONE',  ( -13.10372118337080849, 3.925419760224517329, 6.005889426248455010 ) ) ;
#9133 = LINE ( 'NONE', #7362, #13305 ) ;
#9134 = CARTESIAN_POINT ( 'NONE',  ( -13.39170256340046095, -19.40652054827866380, 5.481861153867630065 ) ) ;
#9135 = EDGE_CURVE ( 'NONE', #14087, #4081, #1140, .T. ) ;
#9136 = CARTESIAN_POINT ( 'NONE',  ( -6.313547257480587760, 11.64110105645932691, 10.00000000000000000 ) ) ;
#9137 = CARTESIAN_POINT ( 'NONE',  ( 0.000000000000000000, 9.000000000000001776, 1.000000000000000000 ) ) ;
#9138 = DIRECTION ( 'NONE',  ( 0.000000000000000000, -0.000000000000000000, 1.000000000000000000 ) ) ;
#9139 = CARTESIAN_POINT ( 'NONE',  ( 11.99178095869207006, 0.000000000000000000, 1.000000000000000000 ) ) ;
#9140 = PLANE ( 'NONE',  #17316 ) ;
#9141 = CARTESIAN_POINT ( 'NONE',  ( -12.52780858231679773, -24.47900456129166358, 4.586221378810390270 ) ) ;
#9142 = CARTESIAN_POINT ( 'NONE',  ( -0.5631383031621635116, -9.114917468222230923, 1.622643865078341463 ) ) ;
#9143 = EDGE_LOOP ( 'NONE', ( #2250, #4615, #292, #17691 ) ) ;
#9144 = CARTESIAN_POINT ( 'NONE',  ( -13.84074239313819277, 4.019990853478630832, 5.241358430878110930 ) ) ;
#9145 = FACE_OUTER_BOUND ( 'NONE', #7154, .T. ) ;
#9146 = ADVANCED_FACE ( 'NONE', ( #919 ), #7306, .T. ) ;
#9147 = CARTESIAN_POINT ( 'NONE',  ( 12.44094141768317741, -20.19639159124061933, 1.768074502826635586 ) ) ;
#9148 = CARTESIAN_POINT ( 'NONE',  ( -5.128441417683177406, -20.99999999999999645, 3.550687472877664952 ) ) ;
#9149 = ORIENTED_EDGE ( 'NONE', *, *, #15120, .T. ) ;
#9150 = EDGE_CURVE ( 'NONE', #1608, #4154, #18710, .T. ) ;
#9151 = CARTESIAN_POINT ( 'NONE',  ( 13.86470821076586368, 4.480264643675554659, 5.874551681240599343 ) ) ;
#9152 = CARTESIAN_POINT ( 'NONE',  ( 12.62499999999998224, -20.24999999999998934, 4.166666666666636765 ) ) ;
#9153 = ORIENTED_EDGE ( 'NONE', *, *, #9098, .T. ) ;
#9154 = ORIENTED_EDGE ( 'NONE', *, *, #16928, .T. ) ;
#9155 = LINE ( 'NONE', #10930, #797 ) ;
#9156 = ORIENTED_EDGE ( 'NONE', *, *, #7798, .T. ) ;
#9157 = CARTESIAN_POINT ( 'NONE',  ( -13.87406079471522347, 4.952570133121557028, 5.260711232101737522 ) ) ;
#9158 = CARTESIAN_POINT ( 'NONE',  ( 0.000000000000000000, -9.114917468222230923, 2.372643865078340575 ) ) ;
#9159 = ORIENTED_EDGE ( 'NONE', *, *, #310, .F. ) ;
#9160 = LINE ( 'NONE', #1214, #15960 ) ;
#9161 = PLANE ( 'NONE',  #315 ) ;
#9162 = DIRECTION ( 'NONE',  ( 0.000000000000000000, 0.000000000000000000, 1.000000000000000000 ) ) ;
#9163 = CARTESIAN_POINT ( 'NONE',  ( 2.739050625766161762, -9.875938058683834342, 1.818089155622620412 ) ) ;
#9164 = FACE_OUTER_BOUND ( 'NONE', #4750, .T. ) ;
#9165 = DIRECTION ( 'NONE',  ( -1.000000000000000000, 0.000000000000000000, 0.000000000000000000 ) ) ;
#9166 = LINE ( 'NONE', #12503, #18328 ) ;
#9167 = CARTESIAN_POINT ( 'NONE',  ( 21.17243175760212637, 4.999999999999999112, 1.000000000000000000 ) ) ;
#9168 = CARTESIAN_POINT ( 'NONE',  ( 27.50000000000000711, 4.999999999999999112, 0.000000000000000000 ) ) ;
#9169 = CARTESIAN_POINT ( 'NONE',  ( 13.09030858231679417, -21.63647391050454871, 2.479004561291657804 ) ) ;
#9170 = CARTESIAN_POINT ( 'NONE',  ( -13.12119116326504908, 4.807653744879115010, 5.626470997801169105 ) ) ;
#9171 = CARTESIAN_POINT ( 'NONE',  ( -11.30905858231679595, -22.74294823697954016, 2.828734674606448785 ) ) ;
#9172 = CARTESIAN_POINT ( 'NONE',  ( -12.25344141768317741, -21.94931252712233061, 0.9999999999999978906 ) ) ;
#9173 = ORIENTED_EDGE ( 'NONE', *, *, #10917, .F. ) ;
#9174 = CARTESIAN_POINT ( 'NONE',  ( 13.09560264576187905, 4.265433610975056133, 4.666666666666618113 ) ) ;
#9175 = LINE ( 'NONE', #12820, #7374 ) ;
#9176 = ORIENTED_EDGE ( 'NONE', *, *, #18360, .F. ) ;
#9177 = FACE_OUTER_BOUND ( 'NONE', #5546, .T. ) ;
#9178 = ORIENTED_EDGE ( 'NONE', *, *, #7355, .T. ) ;
#9179 = CARTESIAN_POINT ( 'NONE',  ( 1.619022621591186928, -9.864917468222230923, 2.372643865078341019 ) ) ;
#9180 = VERTEX_POINT ( 'NONE', #2590 ) ;
#9181 = LINE ( 'NONE', #10864, #5298 ) ;
#9182 = EDGE_CURVE ( 'NONE', #95, #14476, #8975, .T. ) ;
#9183 = DIRECTION ( 'NONE',  ( 0.000000000000000000, 0.000000000000000000, 1.000000000000000000 ) ) ;
#9184 = CARTESIAN_POINT ( 'NONE',  ( -0.9854920305337622199, -9.864917468222230923, 1.622643865078341907 ) ) ;
#9185 = FACE_OUTER_BOUND ( 'NONE', #11874, .T. ) ;
#9186 = LINE ( 'NONE', #1243, #9383 ) ;
#9187 = DIRECTION ( 'NONE',  ( 0.000000000000000000, -0.000000000000000000, 1.000000000000000000 ) ) ;
#9188 = CARTESIAN_POINT ( 'NONE',  ( 8.315941417683177406, -20.26807450282663225, 5.303608408759377113 ) ) ;
#9189 = DIRECTION ( 'NONE',  ( 0.000000000000000000, -1.000000000000000000, 0.000000000000000000 ) ) ;
#9190 = CARTESIAN_POINT ( 'NONE',  ( -10.94094141768317741, -20.72672167713052715, 2.298404588716546293 ) ) ;
#9191 = ORIENTED_EDGE ( 'NONE', *, *, #14872, .F. ) ;
#9192 = CARTESIAN_POINT ( 'NONE',  ( 6.152808582316793284, -21.22443879296942626, 5.229004561291659137 ) ) ;
#9193 = LINE ( 'NONE', #20294, #14083 ) ;
#9194 = CARTESIAN_POINT ( 'NONE',  ( -13.85956729540471066, 3.470648417939721231, 6.731609435864099211 ) ) ;
#9195 = VERTEX_POINT ( 'NONE', #12215 ) ;
#9196 = CARTESIAN_POINT ( 'NONE',  ( 12.05905858231679417, -20.72672167713054137, 4.701595411283463477 ) ) ;
#9197 = DIRECTION ( 'NONE',  ( 0.000000000000000000, 0.000000000000000000, 1.000000000000000000 ) ) ;
#9198 = EDGE_LOOP ( 'NONE', ( #16935, #14004, #6688, #5641, #6486 ) ) ;
#9199 = ORIENTED_EDGE ( 'NONE', *, *, #10142, .T. ) ;
#9200 = CARTESIAN_POINT ( 'NONE',  ( 13.67732412376249052, -5.732631749971324631, 6.533692769198849781 ) ) ;
#9201 = VECTOR ( 'NONE', #9421, 1000.000000000000000 ) ;
#9202 = DIRECTION ( 'NONE',  ( 0.000000000000000000, 0.000000000000000000, 1.000000000000000000 ) ) ;
#9203 = VECTOR ( 'NONE', #16970, 1000.000000000000000 ) ;
#9204 = SURFACE_SIDE_STYLE ('',( #3136 ) ) ;
#9205 = ORIENTED_EDGE ( 'NONE', *, *, #19788, .F. ) ;
#9206 = CARTESIAN_POINT ( 'NONE',  ( 17.12779268661489596, 10.00000000000000000, 1.000000000000000000 ) ) ;
#9207 = ORIENTED_EDGE ( 'NONE', *, *, #15684, .T. ) ;
#9208 = LINE ( 'NONE', #1062, #15316 ) ;
#9209 = CARTESIAN_POINT ( 'NONE',  ( 15.50000000000000178, -20.99999999999999645, 1.000000000000000000 ) ) ;
#9210 = DIRECTION ( 'NONE',  ( 1.000000000000000000, 0.000000000000000000, 0.000000000000000000 ) ) ;
#9211 = CARTESIAN_POINT ( 'NONE',  ( 2.768424032093183662, -10.00067216410020166, 1.850123365707658785 ) ) ;
#9212 = ADVANCED_FACE ( 'NONE', ( #179 ), #7920, .T. ) ;
#9213 = CARTESIAN_POINT ( 'NONE',  ( -13.49999999999998401, -18.49999999999999645, 1.000000000000000000 ) ) ;
#9214 = CARTESIAN_POINT ( 'NONE',  ( -13.09358652029869141, 4.163619275088517035, 5.207983256689002083 ) ) ;
#9215 = CARTESIAN_POINT ( 'NONE',  ( 9.340308582316794173, -22.67418626127525982, 5.270995438708342640 ) ) ;
#9216 = CARTESIAN_POINT ( 'NONE',  ( -13.71569110726703045, -3.795099083046435506, 6.575359435862661250 ) ) ;
#9217 = LINE ( 'NONE', #15182, #8371 ) ;
#9218 = CARTESIAN_POINT ( 'NONE',  ( 5.215308582316795949, -23.02099543870833998, 3.136473910504556262 ) ) ;
#9219 = EDGE_CURVE ( 'NONE', #13278, #13849, #1647, .T. ) ;
#9220 = CARTESIAN_POINT ( 'NONE',  ( 11.22219141768317741, -21.02099543870834353, 3.964901035250761208 ) ) ;
#9221 = CARTESIAN_POINT ( 'NONE',  ( -4.840308582316793284, -22.67418626127525982, 5.270995438708342640 ) ) ;
#9222 = ORIENTED_EDGE ( 'NONE', *, *, #9030, .T. ) ;
#9223 = CARTESIAN_POINT ( 'NONE',  ( 13.37499999999998224, -19.49999999999998934, 4.166666666666637653 ) ) ;
#9224 = DIRECTION ( 'NONE',  ( 0.000000000000000000, 0.000000000000000000, -1.000000000000000000 ) ) ;
#9225 = ORIENTED_EDGE ( 'NONE', *, *, #8253, .F. ) ;
#9226 = ORIENTED_EDGE ( 'NONE', *, *, #5357, .T. ) ;
#9227 = PLANE ( 'NONE',  #6453 ) ;
#9228 = VECTOR ( 'NONE', #9464, 1000.000000000000000 ) ;
#9229 = CARTESIAN_POINT ( 'NONE',  ( -12.64751377014909828, -19.11305460747000495, 5.510446717915143289 ) ) ;
#9230 = CARTESIAN_POINT ( 'NONE',  ( -2.534747216115884161, -9.671180236796224960, 2.515503256513427210 ) ) ;
#9231 = CARTESIAN_POINT ( 'NONE',  ( -13.39902456816392906, -19.03675930772010361, 5.497554699623231400 ) ) ;
#9232 = EDGE_CURVE ( 'NONE', #16322, #4631, #9493, .T. ) ;
#9233 = PLANE ( 'NONE',  #714 ) ;
#9234 = DIRECTION ( 'NONE',  ( 0.000000000000000000, -1.000000000000000000, 0.000000000000000000 ) ) ;
#9235 = CARTESIAN_POINT ( 'NONE',  ( 0.000000000000000000, 4.999999999999999112, 1.000000000000000000 ) ) ;
#9236 = LINE ( 'NONE', #9139, #3382 ) ;
#9237 = CARTESIAN_POINT ( 'NONE',  ( 4.647268150593999003, -21.47219718316376458, 5.373337411135923780 ) ) ;
#9238 = CARTESIAN_POINT ( 'NONE',  ( -12.43405858231679595, -23.73192549717337130, 5.303608408759367343 ) ) ;
#9239 = CARTESIAN_POINT ( 'NONE',  ( -0.2815691515810352374, -8.364917468222230923, 1.622643865078524428 ) ) ;
#9240 = EDGE_CURVE ( 'NONE', #7887, #18614, #4970, .T. ) ;
#9241 = ORIENTED_EDGE ( 'NONE', *, *, #8447, .F. ) ;
#9242 = ADVANCED_FACE ( 'NONE', ( #7823 ), #20594, .T. ) ;
#9243 = CARTESIAN_POINT ( 'NONE',  ( -13.84476264919594612, 4.223013784394161974, 5.079233071712400793 ) ) ;
#9244 = CARTESIAN_POINT ( 'NONE',  ( 8.126396343307449754, 10.00000000000000000, 1.000000000000000000 ) ) ;
#9245 = CARTESIAN_POINT ( 'NONE',  ( 10.00344141768317741, -22.05068747287766229, 6.000000000000001776 ) ) ;
#9246 = CARTESIAN_POINT ( 'NONE',  ( -5.315941417683176518, -21.32873467460645145, 4.242948236979555254 ) ) ;
#9247 = VERTEX_POINT ( 'NONE', #11260 ) ;
#9248 = CARTESIAN_POINT ( 'NONE',  ( 13.87470602645761986, 4.985154336109792972, 4.333333333333382775 ) ) ;
#9249 = CARTESIAN_POINT ( 'NONE',  ( -13.67791111847408025, 9.000000000000001776, 0.000000000000000000 ) ) ;
#9250 = EDGE_LOOP ( 'NONE', ( #14002, #3509, #8326, #2906 ) ) ;
#9251 = EDGE_LOOP ( 'NONE', ( #10002, #17868, #18883, #17171 ) ) ;
#9252 = CARTESIAN_POINT ( 'NONE',  ( -21.42243175760212637, 0.000000000000000000, 0.000000000000000000 ) ) ;
#9253 = ORIENTED_EDGE ( 'NONE', *, *, #784, .T. ) ;
#9254 = CARTESIAN_POINT ( 'NONE',  ( -13.39722611581222189, -19.12758115148224647, 5.495601574623241170 ) ) ;
#9255 = CARTESIAN_POINT ( 'NONE',  ( -14.49999999999998579, -24.49999999999999289, 4.000000000000000000 ) ) ;
#9256 = AXIS2_PLACEMENT_3D ( 'NONE', #849, #5869, #13698 ) ;
#9257 = ORIENTED_EDGE ( 'NONE', *, *, #6815, .F. ) ;
#9258 = DIRECTION ( 'NONE',  ( 0.000000000000000000, 1.000000000000000000, -0.000000000000000000 ) ) ;
#9259 = CARTESIAN_POINT ( 'NONE',  ( 2.594671182134835163, -9.923034775318452461, 2.580184533305832861 ) ) ;
#9260 = EDGE_CURVE ( 'NONE', #14806, #20584, #3296, .T. ) ;
#9261 = LINE ( 'NONE', #8950, #20021 ) ;
#9262 = CARTESIAN_POINT ( 'NONE',  ( 3.475298211275419380, -9.785109117490691233, 1.987377451789144933 ) ) ;
#9263 = DIRECTION ( 'NONE',  ( 1.000000000000000000, 0.000000000000000000, 0.000000000000000000 ) ) ;
#9264 = CARTESIAN_POINT ( 'NONE',  ( 13.12529397354238192, 5.014845663890295846, 4.791666666666685614 ) ) ;
#9265 = CARTESIAN_POINT ( 'NONE',  ( 14.49999999999998579, -21.99999999999999645, 11.00000000000000178 ) ) ;
#9266 = DIRECTION ( 'NONE',  ( 0.000000000000000000, -0.000000000000000000, 1.000000000000000000 ) ) ;
#9267 = DIRECTION ( 'NONE',  ( -0.000000000000000000, -0.000000000000000000, -1.000000000000000000 ) ) ;
#9268 = CARTESIAN_POINT ( 'NONE',  ( 8.503441417683177406, -22.05068747287766229, 4.499999999999999112 ) ) ;
#9269 = CARTESIAN_POINT ( 'NONE',  ( -13.12529418130016445, 5.014856155665242454, 4.958178834604180629 ) ) ;
#9270 = CARTESIAN_POINT ( 'NONE',  ( -8.402808582316797725, -22.46490103525074034, 2.520995438708341307 ) ) ;
#9271 = CARTESIAN_POINT ( 'NONE',  ( -6.065941417683177406, -23.73192549717336064, 1.696391591240623331 ) ) ;
#9272 = ORIENTED_EDGE ( 'NONE', *, *, #8397, .T. ) ;
#9273 = CARTESIAN_POINT ( 'NONE',  ( 13.37680511754115287, -19.40884156416817774, 4.692171866446762429 ) ) ;
#9274 = CARTESIAN_POINT ( 'NONE',  ( -14.49999999999998579, -24.49999999999999289, 1.000000000000000000 ) ) ;
#9275 = ORIENTED_EDGE ( 'NONE', *, *, #6410, .F. ) ;
#9276 = EDGE_CURVE ( 'NONE', #6794, #12837, #14186, .T. ) ;
#9277 = CARTESIAN_POINT ( 'NONE',  ( -20.75349085826862350, 10.00000000000000000, 1.000000000000000000 ) ) ;
#9278 = ORIENTED_EDGE ( 'NONE', *, *, #5646, .T. ) ;
#9279 = CARTESIAN_POINT ( 'NONE',  ( 1.743623630681728542, -9.116095536440919744, 2.372946416531167557 ) ) ;
#9280 = ORIENTED_EDGE ( 'NONE', *, *, #13629, .F. ) ;
#9281 = CARTESIAN_POINT ( 'NONE',  ( 3.499999999999998668, -19.50000000000000000, 1.000000000000000000 ) ) ;
#9282 = CARTESIAN_POINT ( 'NONE',  ( -7.869520639128047002, 0.000000000000000000, 1.000000000000000000 ) ) ;
#9283 = ADVANCED_FACE ( 'NONE', ( #1344 ), #11168, .T. ) ;
#9284 = EDGE_CURVE ( 'NONE', #14996, #6964, #11892, .T. ) ;
#9285 = CARTESIAN_POINT ( 'NONE',  ( -2.081625295426255295, -10.37614485793134556, 1.753937271548854815 ) ) ;
#9286 = CARTESIAN_POINT ( 'NONE',  ( 8.876396343307449754, 0.000000000000000000, 1.000000000000000000 ) ) ;
#9287 = DIRECTION ( 'NONE',  ( 0.000000000000000000, -1.000000000000000000, 0.000000000000000000 ) ) ;
#9288 = VECTOR ( 'NONE', #20164, 1000.000000000000227 ) ;
#9289 = CARTESIAN_POINT ( 'NONE',  ( 21.17243175760212637, 0.000000000000000000, 1.000000000000000000 ) ) ;
#9290 = CARTESIAN_POINT ( 'NONE',  ( 3.974842109207560537, -21.73478823434188456, 6.006404853634143670 ) ) ;
#9291 = FACE_OUTER_BOUND ( 'NONE', #2493, .T. ) ;
#9292 = AXIS2_PLACEMENT_3D ( 'NONE', #16610, #10559, #20091 ) ;
#9293 = CARTESIAN_POINT ( 'NONE',  ( -8.972191417683177406, -23.72900456129165292, 2.724438792969417822 ) ) ;
#9294 = ORIENTED_EDGE ( 'NONE', *, *, #9045, .F. ) ;
#9295 = CARTESIAN_POINT ( 'NONE',  ( 13.27780858231679417, -19.52099543870833642, 2.413778621189609286 ) ) ;
#9296 = CARTESIAN_POINT ( 'NONE',  ( -11.00000000000000000, -25.49999999999999645, 4.000000000000000000 ) ) ;
#9297 = CARTESIAN_POINT ( 'NONE',  ( -13.90434039801927568, 5.731690099970989216, 5.115558489342345361 ) ) ;
#9298 = ORIENTED_EDGE ( 'NONE', *, *, #2983, .T. ) ;
#9299 = ADVANCED_FACE ( 'NONE', ( #20497 ), #6245, .T. ) ;
#9300 = CARTESIAN_POINT ( 'NONE',  ( 6.902808582316793284, -22.77556120703056308, 1.770995438708339975 ) ) ;
#9301 = DIRECTION ( 'NONE',  ( -2.312964634635756072E-15, 1.000000000000000000, 0.000000000000000000 ) ) ;
#9302 = ORIENTED_EDGE ( 'NONE', *, *, #14474, .F. ) ;
#9303 = CARTESIAN_POINT ( 'NONE',  ( 13.37923893525309715, -20.78593376972237650, 5.366589449429977954 ) ) ;
#9304 = CARTESIAN_POINT ( 'NONE',  ( 13.42791111847407848, 0.000000000000000000, 0.000000000000000000 ) ) ;
#9305 =( NAMED_UNIT ( * ) SI_UNIT ( $, .STERADIAN. ) SOLID_ANGLE_UNIT ( ) );
#9306 = ORIENTED_EDGE ( 'NONE', *, *, #1609, .F. ) ;
#9307 = AXIS2_PLACEMENT_3D ( 'NONE', #6134, #4247, #2792 ) ;
#9308 = LINE ( 'NONE', #8159, #5788 ) ;
#9309 = AXIS2_PLACEMENT_3D ( 'NONE', #14914, #6976, #5196 ) ;
#9310 = ORIENTED_EDGE ( 'NONE', *, *, #8649, .F. ) ;
#9311 = CARTESIAN_POINT ( 'NONE',  ( -13.27780858231679595, -20.27099543870833642, 2.724438792969431589 ) ) ;
#9312 = CARTESIAN_POINT ( 'NONE',  ( 12.62500000000001954, -20.25000000000274269, 4.083333333315724012 ) ) ;
#9313 = CARTESIAN_POINT ( 'NONE',  ( 3.187906586576829682, -9.105473976199601083, 1.812833570429532859 ) ) ;
#9314 = DIRECTION ( 'NONE',  ( -0.000000000000000000, 0.000000000000000000, -1.000000000000000000 ) ) ;
#9315 = CARTESIAN_POINT ( 'NONE',  ( -13.37818000216760694, -19.33940989053615311, 4.728953261990445966 ) ) ;
#9316 = VECTOR ( 'NONE', #2030, 1000.000000000000000 ) ;
#9317 = CARTESIAN_POINT ( 'NONE',  ( 8.590308582316794173, -21.32581373872472597, 1.729004561291657582 ) ) ;
#9318 = CARTESIAN_POINT ( 'NONE',  ( -13.87824226375436965, 4.413734319597230282, 6.694665752684481497 ) ) ;
#9319 = VECTOR ( 'NONE', #16834, 1000.000000000000000 ) ;
#9320 = CARTESIAN_POINT ( 'NONE',  ( 0.000000000000000000, 9.000000000000001776, 0.000000000000000000 ) ) ;
#9321 = CARTESIAN_POINT ( 'NONE',  ( 9.340308582316794173, -22.67418626127525982, 5.270995438708342640 ) ) ;
#9322 = EDGE_CURVE ( 'NONE', #10774, #12491, #18917, .T. ) ;
#9323 = CARTESIAN_POINT ( 'NONE',  ( 12.99655858231679595, -22.05068747287764452, 2.499999999999999112 ) ) ;
#9324 = ORIENTED_EDGE ( 'NONE', *, *, #14510, .F. ) ;
#9325 = CARTESIAN_POINT ( 'NONE',  ( 13.41806913471718588, -17.32500869677464550, 4.784333296715663764 ) ) ;
#9326 = DIRECTION ( 'NONE',  ( 0.000000000000000000, -0.000000000000000000, -1.000000000000000000 ) ) ;
#9327 = ORIENTED_EDGE ( 'NONE', *, *, #17304, .T. ) ;
#9328 = EDGE_CURVE ( 'NONE', #14057, #12443, #11071, .T. ) ;
#9329 = ORIENTED_EDGE ( 'NONE', *, *, #12776, .F. ) ;
#9330 = FACE_OUTER_BOUND ( 'NONE', #7294, .T. ) ;
#9331 = AXIS2_PLACEMENT_3D ( 'NONE', #15296, #14038, #18765 ) ;
#9332 = CARTESIAN_POINT ( 'NONE',  ( -12.65051119073526564, -18.96168486786632457, 5.513701926248478102 ) ) ;
#9333 = VECTOR ( 'NONE', #18083, 1000.000000000000000 ) ;
#9334 = CARTESIAN_POINT ( 'NONE',  ( -2.616191246582922680, -8.630616848980537270, 2.440880773935528048 ) ) ;
#9335 = CARTESIAN_POINT ( 'NONE',  ( -13.39296152110871851, -19.34294318400601753, 5.489418334493660012 ) ) ;
#9336 = DIRECTION ( 'NONE',  ( 1.000000000000000000, 0.000000000000000000, 0.000000000000000000 ) ) ;
#9337 = DIRECTION ( 'NONE',  ( 0.000000000000000000, 1.000000000000000000, 0.000000000000000000 ) ) ;
#9338 = CARTESIAN_POINT ( 'NONE',  ( 11.68405858231679417, -20.79840458871652942, 2.226721677130544030 ) ) ;
#9339 = DIRECTION ( 'NONE',  ( 0.000000000000000000, 0.000000000000000000, 1.000000000000000000 ) ) ;
#9340 = CARTESIAN_POINT ( 'NONE',  ( 13.12519991495504712, 4.260095705229160146, 6.739971950528219402 ) ) ;
#9341 = CARTESIAN_POINT ( 'NONE',  ( -5.402808582316795949, -23.08622137881038938, 1.020995438708339309 ) ) ;
#9342 = CARTESIAN_POINT ( 'NONE',  ( -1.872293763630120678, -10.04602735435188698, 2.419156501869924369 ) ) ;
#9343 = ORIENTED_EDGE ( 'NONE', *, *, #18783, .T. ) ;
#9344 = CARTESIAN_POINT ( 'NONE',  ( -13.37499999999998224, -20.24999999999998934, 4.166666666666636765 ) ) ;
#9345 = CARTESIAN_POINT ( 'NONE',  ( -20.00000000000000000, 0.000000000000000000, 0.5000000000000000000 ) ) ;
#9346 = CARTESIAN_POINT ( 'NONE',  ( 10.19094141768317741, -23.80360840875937001, 5.231925497173365081 ) ) ;
#9347 = CARTESIAN_POINT ( 'NONE',  ( -7.003441417683177406, -22.05068747287766229, 4.499999999999999112 ) ) ;
#9348 = VECTOR ( 'NONE', #14443, 1000.000000000000000 ) ;
#9349 = ORIENTED_EDGE ( 'NONE', *, *, #9284, .T. ) ;
#9350 = CARTESIAN_POINT ( 'NONE',  ( 13.41834698511420676, -18.81097725173551893, 6.252442769197418926 ) ) ;
#9351 = LINE ( 'NONE', #19093, #8389 ) ;
#9352 = ORIENTED_EDGE ( 'NONE', *, *, #2961, .T. ) ;
#9353 = PLANE ( 'NONE',  #15779 ) ;
#9354 = AXIS2_PLACEMENT_3D ( 'NONE', #10036, #208, #8474 ) ;
#9355 = EDGE_CURVE ( 'NONE', #18598, #12925, #10962, .T. ) ;
#9356 = ORIENTED_EDGE ( 'NONE', *, *, #9874, .F. ) ;
#9357 = CARTESIAN_POINT ( 'NONE',  ( -13.39662663169496781, -19.15785509940297615, 5.494950532956567102 ) ) ;
#9358 = CARTESIAN_POINT ( 'NONE',  ( 7.499999999999999112, -25.49999999999999645, 6.500000000000000000 ) ) ;
#9359 = EDGE_CURVE ( 'NONE', #10724, #2654, #9392, .T. ) ;
#9360 = VECTOR ( 'NONE', #8880, 1000.000000000000000 ) ;
#9361 = EDGE_CURVE ( 'NONE', #14781, #7837, #9588, .T. ) ;
#9362 = VERTEX_POINT ( 'NONE', #10865 ) ;
#9363 = CARTESIAN_POINT ( 'NONE',  ( -13.49999999999998401, -21.99999999999999645, 11.68378559369222280 ) ) ;
#9364 = CARTESIAN_POINT ( 'NONE',  ( 2.534747216115884161, -9.671180236796224960, 2.515503256513427210 ) ) ;
#9365 = DIRECTION ( 'NONE',  ( 1.000000000000000000, 0.000000000000000000, 0.000000000000000000 ) ) ;
#9366 = CARTESIAN_POINT ( 'NONE',  ( 1.720709671993384093, -9.114925383610804843, 1.622645897908254753 ) ) ;
#9367 = PLANE ( 'NONE',  #19228 ) ;
#9368 = LINE ( 'NONE', #1621, #413 ) ;
#9369 = AXIS2_PLACEMENT_3D ( 'NONE', #8621, #3710, #10090 ) ;
#9370 = LINE ( 'NONE', #2569, #15661 ) ;
#9371 = CYLINDRICAL_SURFACE ( 'NONE', #2698, 0.5000000000000000000 ) ;
#9372 = LINE ( 'NONE', #3100, #18382 ) ;
#9373 = CARTESIAN_POINT ( 'NONE',  ( 6.440941417683175629, -21.25705176302044208, 2.828734674606458555 ) ) ;
#9374 = CARTESIAN_POINT ( 'NONE',  ( -13.10252221513633941, 3.864871864382954048, 6.004587342915129966 ) ) ;
#9375 = CARTESIAN_POINT ( 'NONE',  ( -9.902808582316795949, -22.46490103525074034, 2.520995438708341307 ) ) ;
#9376 = CARTESIAN_POINT ( 'NONE',  ( -6.815941417683177406, -20.26807450282663225, 5.303608408759377113 ) ) ;
#9377 = ORIENTED_EDGE ( 'NONE', *, *, #11405, .F. ) ;
#9378 = CARTESIAN_POINT ( 'NONE',  ( 13.09556065010287362, 4.263312830196960057, 5.034075356110313315 ) ) ;
#9379 = LINE ( 'NONE', #10857, #8339 ) ;
#9380 = ORIENTED_EDGE ( 'NONE', *, *, #2204, .T. ) ;
#9381 = LINE ( 'NONE', #14180, #11955 ) ;
#9382 = EDGE_CURVE ( 'NONE', #4631, #3772, #2908, .T. ) ;
#9383 = VECTOR ( 'NONE', #9395, 1000.000000000000000 ) ;
#9384 = ORIENTED_EDGE ( 'NONE', *, *, #18821, .F. ) ;
#9385 = CARTESIAN_POINT ( 'NONE',  ( 1.865667289525601680, -9.999006358835732300, 2.407080570882605297 ) ) ;
#9386 = VECTOR ( 'NONE', #8940, 1000.000000000000000 ) ;
#9387 = AXIS2_PLACEMENT_3D ( 'NONE', #9882, #20577, #19210 ) ;
#9388 = VECTOR ( 'NONE', #8926, 1000.000000000000000 ) ;
#9389 = VECTOR ( 'NONE', #6844, 1000.000000000000000 ) ;
#9390 = ORIENTED_EDGE ( 'NONE', *, *, #11641, .T. ) ;
#9391 = CARTESIAN_POINT ( 'NONE',  ( 8.034691417683175629, -20.22900456129164581, 2.825813738724748170 ) ) ;
#9392 = LINE ( 'NONE', #17230, #10665 ) ;
#9393 = CARTESIAN_POINT ( 'NONE',  ( -1.866357130655357688, -10.00562759449716133, 2.408781036472938730 ) ) ;
#9394 = DIRECTION ( 'NONE',  ( 0.000000000000000000, 0.000000000000000000, 1.000000000000000000 ) ) ;
#9395 = DIRECTION ( 'NONE',  ( 1.000000000000000000, 0.000000000000000000, 0.000000000000000000 ) ) ;
#9396 = ADVANCED_FACE ( 'NONE', ( #3015 ), #15764, .T. ) ;
#9397 = CARTESIAN_POINT ( 'NONE',  ( 22.56633994409548194, 11.64110105645932691, 0.000000000000000000 ) ) ;
#9398 = CARTESIAN_POINT ( 'NONE',  ( 12.34719141768317563, -21.22443879296941915, 1.770995438708345748 ) ) ;
#9399 = FILL_AREA_STYLE ('',( #20703 ) ) ;
#9400 = CARTESIAN_POINT ( 'NONE',  ( -6.909691417683177406, -21.32581373872474373, 5.270995438708348857 ) ) ;
#9401 = VECTOR ( 'NONE', #9447, 1000.000000000000000 ) ;
#9402 = VERTEX_POINT ( 'NONE', #3621 ) ;
#9403 = CARTESIAN_POINT ( 'NONE',  ( 6.434058582316794173, -23.20159541128345992, 4.773278322869455970 ) ) ;
#9404 = CARTESIAN_POINT ( 'NONE',  ( -9.999999999999998224, -30.00000000000000355, 0.000000000000000000 ) ) ;
#9405 = CARTESIAN_POINT ( 'NONE',  ( -12.62527129584495000, -20.98629955982801576, 4.726243163759704657 ) ) ;
#9406 = ORIENTED_EDGE ( 'NONE', *, *, #7691, .F. ) ;
#9407 = DIRECTION ( 'NONE',  ( 1.000000000000000000, 0.000000000000000000, 0.000000000000000000 ) ) ;
#9408 = EDGE_CURVE ( 'NONE', #12390, #13746, #15012, .T. ) ;
#9409 = DIRECTION ( 'NONE',  ( -0.000000000000000000, 0.000000000000000000, -1.000000000000000000 ) ) ;
#9410 = EDGE_CURVE ( 'NONE', #9650, #19732, #14601, .T. ) ;
#9411 = VERTEX_POINT ( 'NONE', #19633 ) ;
#9412 = CARTESIAN_POINT ( 'NONE',  ( 13.87500000000000000, 5.000000000000049738, 4.000000000000001776 ) ) ;
#9413 = ORIENTED_EDGE ( 'NONE', *, *, #17219, .T. ) ;
#9414 = EDGE_CURVE ( 'NONE', #10619, #12385, #14814, .T. ) ;
#9415 = CARTESIAN_POINT ( 'NONE',  ( -15.49999999999999822, -22.99999999999999289, 4.000000000000000000 ) ) ;
#9416 = VERTEX_POINT ( 'NONE', #16382 ) ;
#9417 = CARTESIAN_POINT ( 'NONE',  ( -11.96530858231679595, -20.22900456129164937, 4.174186261275266929 ) ) ;
#9418 = VECTOR ( 'NONE', #12125, 1000.000000000000000 ) ;
#9419 = CARTESIAN_POINT ( 'NONE',  ( 12.64131715375063258, -19.42598373559290792, 5.491151580003103660 ) ) ;
#9420 = VECTOR ( 'NONE', #5710, 1000.000000000000000 ) ;
#9421 = DIRECTION ( 'NONE',  ( -0.000000000000000000, 1.000000000000000000, -0.000000000000000000 ) ) ;
#9422 = CARTESIAN_POINT ( 'NONE',  ( 0.5631383031621635116, -9.864917468222230923, 1.622643865078341907 ) ) ;
#9423 = ADVANCED_FACE ( 'NONE', ( #5402 ), #14911, .F. ) ;
#9424 = CARTESIAN_POINT ( 'NONE',  ( -23.35856191738413656, 9.000000000000001776, 1.000000000000000000 ) ) ;
#9425 = CARTESIAN_POINT ( 'NONE',  ( -13.68663801924254741, -3.762280028282741551, 5.075999963380942503 ) ) ;
#9426 = CARTESIAN_POINT ( 'NONE',  ( 4.934058582316793284, -23.20159541128345992, 4.773278322869455970 ) ) ;
#9427 = CARTESIAN_POINT ( 'NONE',  ( -12.66024186180961308, -19.22028597861421417, 6.258173329156003106 ) ) ;
#9428 = CARTESIAN_POINT ( 'NONE',  ( -13.17791111847408025, 9.000000000000001776, 1.000000000000000000 ) ) ;
#9429 = CARTESIAN_POINT ( 'NONE',  ( 8.121558582316792396, -23.74999999999999645, 3.550687472877651629 ) ) ;
#9430 = CARTESIAN_POINT ( 'NONE',  ( 6.440941417683175629, -21.25705176302044208, 2.828734674606458555 ) ) ;
#9431 = CARTESIAN_POINT ( 'NONE',  ( -6.715308582316794173, -23.77099543870833998, 2.825813738724734847 ) ) ;
#9432 = VERTEX_POINT ( 'NONE', #11774 ) ;
#9433 = CARTESIAN_POINT ( 'NONE',  ( 13.37499999998404299, -19.49999999996810729, 2.793053905886972998 ) ) ;
#9434 = CARTESIAN_POINT ( 'NONE',  ( -2.506848361495492394, -9.459347215042898327, 1.711100304737409150 ) ) ;
#9435 = ORIENTED_EDGE ( 'NONE', *, *, #4414, .F. ) ;
#9436 = ORIENTED_EDGE ( 'NONE', *, *, #13064, .F. ) ;
#9437 = LINE ( 'NONE', #15810, #9442 ) ;
#9438 = VECTOR ( 'NONE', #18211, 1000.000000000000000 ) ;
#9439 = LINE ( 'NONE', #1489, #14937 ) ;
#9440 = CARTESIAN_POINT ( 'NONE',  ( -0.2815691515810352374, -8.364917468222230923, 2.372643865078523540 ) ) ;
#9441 = LINE ( 'NONE', #3067, #2671 ) ;
#9442 = VECTOR ( 'NONE', #19067, 1000.000000000000000 ) ;
#9443 = EDGE_CURVE ( 'NONE', #6572, #18339, #20365, .T. ) ;
#9444 = LINE ( 'NONE', #4937, #14051 ) ;
#9445 = LINE ( 'NONE', #2647, #5197 ) ;
#9446 = CARTESIAN_POINT ( 'NONE',  ( 10.09030858231679417, -21.32581373872472952, 1.729004561291657138 ) ) ;
#9447 = DIRECTION ( 'NONE',  ( 1.000000000000000000, -2.312964634635752916E-15, 0.000000000000000000 ) ) ;
#9448 = CARTESIAN_POINT ( 'NONE',  ( 12.62499979224180180, -20.25001049178813162, 4.458178821399696012 ) ) ;
#9449 = CARTESIAN_POINT ( 'NONE',  ( -12.15969141768317918, -22.98484643305507191, 0.9790045612916508100 ) ) ;
#9450 = CARTESIAN_POINT ( 'NONE',  ( -0.5631383031621635116, -9.864917468222230923, 1.622643865078341907 ) ) ;
#9451 = VERTEX_POINT ( 'NONE', #6667 ) ;
#9452 = CARTESIAN_POINT ( 'NONE',  ( -13.84501469867711698, 4.235742283194553259, 4.333333333333380999 ) ) ;
#9453 = DIRECTION ( 'NONE',  ( 1.000000000000000000, 0.000000000000000000, 0.000000000000000000 ) ) ;
#9454 = CARTESIAN_POINT ( 'NONE',  ( 12.62844141768317741, -20.24999999999999289, 3.550687472877664952 ) ) ;
#9455 = CARTESIAN_POINT ( 'NONE',  ( -11.12155858231679595, -22.99999999999999645, 3.550687472877652073 ) ) ;
#9456 = ORIENTED_EDGE ( 'NONE', *, *, #2878, .T. ) ;
#9457 = CARTESIAN_POINT ( 'NONE',  ( 13.40957725085194241, -19.25384883197511243, 6.242932005802575901 ) ) ;
#9458 = CARTESIAN_POINT ( 'NONE',  ( 12.62499999999998224, -20.25000000000006395, 4.416666666666681174 ) ) ;
#9459 = DIRECTION ( 'NONE',  ( 1.000000000000000000, -0.000000000000000000, 0.000000000000000000 ) ) ;
#9460 = EDGE_LOOP ( 'NONE', ( #4880, #14544, #5191, #13361 ) ) ;
#9461 = VECTOR ( 'NONE', #9107, 1000.000000000000000 ) ;
#9462 = ORIENTED_EDGE ( 'NONE', *, *, #18596, .F. ) ;
#9463 = FACE_OUTER_BOUND ( 'NONE', #10362, .T. ) ;
#9464 = DIRECTION ( 'NONE',  ( 0.000000000000000000, 1.000000000000000000, -0.000000000000000000 ) ) ;
#9465 = ORIENTED_EDGE ( 'NONE', *, *, #14205, .F. ) ;
#9466 = VECTOR ( 'NONE', #15476, 1000.000000000000000 ) ;
#9467 = DIRECTION ( 'NONE',  ( 0.000000000000000000, -0.000000000000000000, 1.000000000000000000 ) ) ;
#9468 = DIRECTION ( 'NONE',  ( 0.000000000000000000, 0.000000000000000000, 1.000000000000000000 ) ) ;
#9469 = PLANE ( 'NONE',  #19037 ) ;
#9470 = CARTESIAN_POINT ( 'NONE',  ( 3.059891148793807414, -12.07002330923453570, 2.381574079220715401 ) ) ;
#9471 = CARTESIAN_POINT ( 'NONE',  ( 10.93924542913430820, 16.00000000000000000, 1.000000000000000000 ) ) ;
#9472 = LINE ( 'NONE', #11451, #18787 ) ;
#9473 = EDGE_CURVE ( 'NONE', #7127, #20463, #17755, .T. ) ;
#9474 = CARTESIAN_POINT ( 'NONE',  ( -7.626396343307448866, 10.00000000000000000, 1.000000000000000000 ) ) ;
#9475 = FACE_OUTER_BOUND ( 'NONE', #374, .T. ) ;
#9476 = LINE ( 'NONE', #19001, #10717 ) ;
#9477 = CARTESIAN_POINT ( 'NONE',  ( -12.62499999999990052, -20.34958158682421114, 3.551156945994469627 ) ) ;
#9478 = CARTESIAN_POINT ( 'NONE',  ( 4.190941417683176518, -22.74294823697955081, 4.171265325393542334 ) ) ;
#9479 = CARTESIAN_POINT ( 'NONE',  ( -13.12424783836753228, 4.962015837561366993, 5.328858059679200565 ) ) ;
#9480 = CARTESIAN_POINT ( 'NONE',  ( -6.715308582316796837, -23.02099543870833998, 3.136473910504556262 ) ) ;
#9481 = CARTESIAN_POINT ( 'NONE',  ( -11.78469141768317563, -23.77099543870834353, 4.174186261275252718 ) ) ;
#9482 = ORIENTED_EDGE ( 'NONE', *, *, #5577, .F. ) ;
#9483 = EDGE_CURVE ( 'NONE', #8532, #19920, #11366, .T. ) ;
#9484 = CARTESIAN_POINT ( 'NONE',  ( 13.09560264576187905, 4.265433610975056133, 2.999999999999999556 ) ) ;
#9485 = DIRECTION ( 'NONE',  ( 0.000000000000000000, 0.000000000000000000, 1.000000000000000000 ) ) ;
#9486 = ORIENTED_EDGE ( 'NONE', *, *, #7079, .T. ) ;
#9487 = ADVANCED_FACE ( 'NONE', ( #6869 ), #587, .T. ) ;
#9488 = DIRECTION ( 'NONE',  ( 4.625929269271486900E-15, 1.000000000000000000, 0.000000000000000000 ) ) ;
#9489 = ORIENTED_EDGE ( 'NONE', *, *, #4119, .F. ) ;
#9490 = CARTESIAN_POINT ( 'NONE',  ( -18.69064177244175795, 10.00000000000000000, 0.000000000000000000 ) ) ;
#9491 = VERTEX_POINT ( 'NONE', #13341 ) ;
#9492 = CARTESIAN_POINT ( 'NONE',  ( 8.597191417683177406, -22.77556120703057729, 5.229004561291656472 ) ) ;
#9493 = LINE ( 'NONE', #12420, #2624 ) ;
#9494 = CARTESIAN_POINT ( 'NONE',  ( -1.717920576997000737, -9.114924032904250240, 2.372645551019823884 ) ) ;
#9495 = LINE ( 'NONE', #18919, #17374 ) ;
#9496 = LINE ( 'NONE', #12832, #18331 ) ;
#9497 = ADVANCED_FACE ( 'NONE', ( #3831 ), #2157, .T. ) ;
#9498 = CARTESIAN_POINT ( 'NONE',  ( -10.38119784648305632, -14.00000000000000000, 2.000000000000000000 ) ) ;
#9499 = CARTESIAN_POINT ( 'NONE',  ( 7.190941417683177406, -23.80360840875937001, 5.231925497173365081 ) ) ;
#9500 = CARTESIAN_POINT ( 'NONE',  ( -8.597191417683177406, -22.77556120703057729, 5.229004561291655584 ) ) ;
#9501 = ORIENTED_EDGE ( 'NONE', *, *, #16619, .F. ) ;
#9502 = CARTESIAN_POINT ( 'NONE',  ( 6.996558582316793284, -22.05068747287764452, 1.749999999999998446 ) ) ;
#9503 = CARTESIAN_POINT ( 'NONE',  ( 12.62499999999998401, -20.24999999999998934, 2.439580858552613751 ) ) ;
#9504 = CARTESIAN_POINT ( 'NONE',  ( -12.85087781109329974, -9.593170539812428288, 6.465204579154565145 ) ) ;
#9505 = ORIENTED_EDGE ( 'NONE', *, *, #11546, .T. ) ;
#9506 = CARTESIAN_POINT ( 'NONE',  ( 6.152808582316793284, -21.22443879296942626, 5.229004561291659137 ) ) ;
#9507 = ORIENTED_EDGE ( 'NONE', *, *, #13111, .T. ) ;
#9508 = PRODUCT_DEFINITION_SHAPE ( 'NONE', 'NONE',  #20722 ) ;
#9509 = CARTESIAN_POINT ( 'NONE',  ( 25.04469207716615031, 4.999999999999999112, 1.000000000000000000 ) ) ;
#9510 = ORIENTED_EDGE ( 'NONE', *, *, #11019, .F. ) ;
#9511 = LINE ( 'NONE', #6383, #14800 ) ;
#9512 = EDGE_LOOP ( 'NONE', ( #2351, #16990, #9053, #13665 ) ) ;
#9513 = CARTESIAN_POINT ( 'NONE',  ( -6.996558582316793284, -22.05068747287764452, 1.749999999999998446 ) ) ;
#9514 = CARTESIAN_POINT ( 'NONE',  ( -26.19203811574920593, 16.00000000000000000, 1.000000000000000000 ) ) ;
#9515 = DIRECTION ( 'NONE',  ( 1.000000000000000000, 0.000000000000000000, 0.000000000000000000 ) ) ;
#9516 = CARTESIAN_POINT ( 'NONE',  ( 2.557403344953185442, -14.91030650174552896, 3.668400560659690779 ) ) ;
#9517 = EDGE_CURVE ( 'NONE', #2477, #2500, #6970, .T. ) ;
#9518 = EDGE_CURVE ( 'NONE', #12186, #5929, #298, .T. ) ;
#9519 = FACE_OUTER_BOUND ( 'NONE', #6241, .T. ) ;
#9520 = CARTESIAN_POINT ( 'NONE',  ( -13.84402619238587206, 4.185822715484293077, 5.150938132831436533 ) ) ;
#9521 = CARTESIAN_POINT ( 'NONE',  ( 6.715308582316794173, -23.77099543870833998, 2.825813738724734847 ) ) ;
#9522 = CARTESIAN_POINT ( 'NONE',  ( -12.62608183053121458, -20.94536755816881168, 4.949360998036265613 ) ) ;
#9523 = DIRECTION ( 'NONE',  ( -0.000000000000000000, 0.000000000000000000, 1.000000000000000000 ) ) ;
#9524 = CARTESIAN_POINT ( 'NONE',  ( -5.871558582316795949, -19.49999999999998934, 3.449312527122348371 ) ) ;
#9525 = DIRECTION ( 'NONE',  ( 0.000000000000000000, 1.000000000000000000, 0.000000000000000000 ) ) ;
#9526 = VECTOR ( 'NONE', #9258, 1000.000000000000000 ) ;
#9527 = CARTESIAN_POINT ( 'NONE',  ( 5.222191417683177406, -21.02099543870834353, 3.964901035250761208 ) ) ;
#9528 = CARTESIAN_POINT ( 'NONE',  ( -11.22219141768317741, -20.27099543870833998, 4.275561207030583510 ) ) ;
#9529 = ORIENTED_EDGE ( 'NONE', *, *, #12324, .F. ) ;
#9530 = CARTESIAN_POINT ( 'NONE',  ( 13.83051420738022763, 3.503467472703414742, 5.232249963382380464 ) ) ;
#9531 = DIRECTION ( 'NONE',  ( -1.000000000000000000, 0.000000000000000000, 0.000000000000000000 ) ) ;
#9532 = ORIENTED_EDGE ( 'NONE', *, *, #15128, .T. ) ;
#9533 = EDGE_CURVE ( 'NONE', #15883, #19, #19743, .T. ) ;
#9534 = ORIENTED_EDGE ( 'NONE', *, *, #13482, .T. ) ;
#9535 = PLANE ( 'NONE',  #10450 ) ;
#9536 = DIRECTION ( 'NONE',  ( 1.000000000000000000, 0.000000000000000000, -0.000000000000000000 ) ) ;
#9537 = CARTESIAN_POINT ( 'NONE',  ( 20.49999999999998224, -21.99999999999999645, 11.00000000000000178 ) ) ;
#9538 = AXIS2_PLACEMENT_3D ( 'NONE', #495, #3431, #9808 ) ;
#9539 = CARTESIAN_POINT ( 'NONE',  ( -3.549867680106858714, -10.29705900472337632, 2.118856410057032402 ) ) ;
#9540 = DIRECTION ( 'NONE',  ( 1.000000000000000000, 0.000000000000000000, 0.000000000000000000 ) ) ;
#9541 = EDGE_CURVE ( 'NONE', #6861, #5289, #8540, .T. ) ;
#9542 = ADVANCED_FACE ( 'NONE', ( #18165 ), #3424, .T. ) ;
#9543 = LINE ( 'NONE', #14453, #12398 ) ;
#9544 = CARTESIAN_POINT ( 'NONE',  ( -12.62562019941893432, -20.21867992933967173, 4.757612834768309540 ) ) ;
#9545 = CARTESIAN_POINT ( 'NONE',  ( 10.55905858231679595, -20.72672167713054137, 4.701595411283463477 ) ) ;
#9546 = CYLINDRICAL_SURFACE ( 'NONE', #5378, 59.99999999999999289 ) ;
#9547 = CARTESIAN_POINT ( 'NONE',  ( 13.15469878640066526, 5.749788713235649773, 5.232478742873432509 ) ) ;
#9548 = CARTESIAN_POINT ( 'NONE',  ( -2.050137595624097031, -10.15260257655714504, 1.696527147986202522 ) ) ;
#9549 = VERTEX_POINT ( 'NONE', #9802 ) ;
#9550 = CARTESIAN_POINT ( 'NONE',  ( -13.37499999999998401, -20.99999999999999645, 3.146526952850934755 ) ) ;
#9551 = LINE ( 'NONE', #348, #15049 ) ;
#9552 = CARTESIAN_POINT ( 'NONE',  ( 6.909691417683176518, -21.01515356694492098, 6.020995438708349745 ) ) ;
#9553 = CARTESIAN_POINT ( 'NONE',  ( -11.87155858231679595, -20.99999999999999645, 3.449312527122348371 ) ) ;
#9554 = VERTEX_POINT ( 'NONE', #5193 ) ;
#9555 = CARTESIAN_POINT ( 'NONE',  ( 13.37505392270939986, -20.99727690317663686, 4.612442573673130930 ) ) ;
#9556 = CARTESIAN_POINT ( 'NONE',  ( -6.313547257480587760, 10.00000000000000000, 1.000000000000000000 ) ) ;
#9557 = CARTESIAN_POINT ( 'NONE',  ( -0.000000000000000000, 10.00000000000000000, 0.000000000000000000 ) ) ;
#9558 = ORIENTED_EDGE ( 'NONE', *, *, #1362, .T. ) ;
#9559 = EDGE_CURVE ( 'NONE', #12080, #8135, #16186, .T. ) ;
#9560 = VERTEX_POINT ( 'NONE', #8237 ) ;
#9561 = CARTESIAN_POINT ( 'NONE',  ( 9.000000000000000000, -9.999999999999991118, 2.000000000000000000 ) ) ;
#9562 = DIRECTION ( 'NONE',  ( -1.000000000000000000, -1.734723475976807094E-15, 0.000000000000000000 ) ) ;
#9563 = EDGE_LOOP ( 'NONE', ( #1082, #5599, #9997, #76 ) ) ;
#9564 = CARTESIAN_POINT ( 'NONE',  ( 2.645259258103298983, -10.28229522185712241, 2.672449792925449596 ) ) ;
#9565 = CARTESIAN_POINT ( 'NONE',  ( 11.99178095869207006, 0.000000000000000000, 0.000000000000000000 ) ) ;
#9566 = CARTESIAN_POINT ( 'NONE',  ( 1.797685059409938280, -9.880079706704160358, 1.626537830816663588 ) ) ;
#9567 = DIRECTION ( 'NONE',  ( 2.312964634635752916E-15, 1.000000000000000000, -0.000000000000000000 ) ) ;
#9568 = LINE ( 'NONE', #20575, #15768 ) ;
#9569 = CARTESIAN_POINT ( 'NONE',  ( 21.67243175760212637, 4.999999999999999112, 1.000000000000000000 ) ) ;
#9570 = DIRECTION ( 'NONE',  ( -1.000000000000000000, 0.000000000000000000, 0.000000000000000000 ) ) ;
#9571 = DIRECTION ( 'NONE',  ( 0.000000000000000000, -1.000000000000000000, 0.000000000000000000 ) ) ;
#9572 = CARTESIAN_POINT ( 'NONE',  ( -2.559937518207947793, -9.746075135043517079, 2.534737762559237773 ) ) ;
#9573 = CARTESIAN_POINT ( 'NONE',  ( 12.34030858231679773, -22.36352608949544418, 4.520995438708343528 ) ) ;
#9574 = CARTESIAN_POINT ( 'NONE',  ( -12.95145221759166354, -3.764163011652346569, 5.840524842913703552 ) ) ;
#9575 = CARTESIAN_POINT ( 'NONE',  ( -11.02780858231679595, -23.72900456129165647, 4.275561207030568411 ) ) ;
#9576 = CARTESIAN_POINT ( 'NONE',  ( -5.972191417683178294, -24.47900456129165292, 2.413778621189595963 ) ) ;
#9577 = ORIENTED_EDGE ( 'NONE', *, *, #7561, .F. ) ;
#9578 = CARTESIAN_POINT ( 'NONE',  ( 13.04243487821393721, 1.580461349787872782, 5.205428440007538349 ) ) ;
#9579 = SURFACE_STYLE_FILL_AREA ( #17528 ) ;
#9580 = ORIENTED_EDGE ( 'NONE', *, *, #8154, .T. ) ;
#9581 = ORIENTED_EDGE ( 'NONE', *, *, #10655, .T. ) ;
#9582 = CARTESIAN_POINT ( 'NONE',  ( 12.25209451496117197, 0.000000000000000000, 1.000000000000000000 ) ) ;
#9583 = VERTEX_POINT ( 'NONE', #5095 ) ;
#9584 = LINE ( 'NONE', #1642, #3089 ) ;
#9585 = EDGE_CURVE ( 'NONE', #14879, #14595, #1117, .T. ) ;
#9586 = ORIENTED_EDGE ( 'NONE', *, *, #15537, .F. ) ;
#9587 = CARTESIAN_POINT ( 'NONE',  ( 12.34719141768317741, -21.22443879296941915, 1.770995438708345748 ) ) ;
#9588 = LINE ( 'NONE', #4481, #1305 ) ;
#9589 = CARTESIAN_POINT ( 'NONE',  ( -3.277163086644854229, -14.76879761173520578, 3.824673233536266537 ) ) ;
#9590 = CARTESIAN_POINT ( 'NONE',  ( 11.00000000000000000, -23.83493649053891517, 4.999999999999999112 ) ) ;
#9591 = CARTESIAN_POINT ( 'NONE',  ( -12.90280858231679595, -22.77556120703056308, 1.770995438708340197 ) ) ;
#9592 = DIRECTION ( 'NONE',  ( 0.000000000000000000, 1.000000000000000000, -0.000000000000000000 ) ) ;
#9593 = CARTESIAN_POINT ( 'NONE',  ( 7.940941417683175629, -20.19639159124061933, 1.768074502826635586 ) ) ;
#9594 = DIRECTION ( 'NONE',  ( -0.000000000000000000, -0.000000000000000000, -1.000000000000000000 ) ) ;
#9595 = CARTESIAN_POINT ( 'NONE',  ( -6.628441417683176518, -20.24999999999999289, 3.550687472877664952 ) ) ;
#9596 = ORIENTED_EDGE ( 'NONE', *, *, #4376, .T. ) ;
#9597 = CARTESIAN_POINT ( 'NONE',  ( 8.027808582316792396, -23.72900456129165647, 4.275561207030568411 ) ) ;
#9598 = LINE ( 'NONE', #12740, #15756 ) ;
#9599 = CARTESIAN_POINT ( 'NONE',  ( -12.63806878948643231, -20.34002613093225520, 5.891296472647073124 ) ) ;
#9600 = VERTEX_POINT ( 'NONE', #15124 ) ;
#9601 = CARTESIAN_POINT ( 'NONE',  ( 5.871558582316794173, -20.24999999999999289, 3.449312527122348371 ) ) ;
#9602 = DIRECTION ( 'NONE',  ( -0.000000000000000000, -0.000000000000000000, -1.000000000000000000 ) ) ;
#9603 = ORIENTED_EDGE ( 'NONE', *, *, #2244, .F. ) ;
#9604 = CARTESIAN_POINT ( 'NONE',  ( 13.00000000000000355, 7.806255641895631925E-15, 2.000000000000000000 ) ) ;
#9605 = ORIENTED_EDGE ( 'NONE', *, *, #17075, .T. ) ;
#9606 = EDGE_CURVE ( 'NONE', #12439, #4026, #5818, .T. ) ;
#9607 = LINE ( 'NONE', #9415, #15129 ) ;
#9608 = VERTEX_POINT ( 'NONE', #13546 ) ;
#9609 = CARTESIAN_POINT ( 'NONE',  ( -4.840308582316793284, -22.67418626127525982, 5.270995438708342640 ) ) ;
#9610 = CARTESIAN_POINT ( 'NONE',  ( 12.64751377014909828, -19.11305460747000495, 5.510446717915143289 ) ) ;
#9611 = EDGE_CURVE ( 'NONE', #12804, #20155, #3929, .T. ) ;
#9612 = CARTESIAN_POINT ( 'NONE',  ( 0.000000000000000000, 9.000000000000001776, 1.000000000000000000 ) ) ;
#9613 = CARTESIAN_POINT ( 'NONE',  ( 1.619022621591186928, -9.864917468222230923, 1.622643865078341907 ) ) ;
#9614 = EDGE_CURVE ( 'NONE', #10698, #1939, #6330, .T. ) ;
#9615 = AXIS2_PLACEMENT_3D ( 'NONE', #12016, #11910, #13579 ) ;
#9616 = LINE ( 'NONE', #8065, #12351 ) ;
#9617 = CARTESIAN_POINT ( 'NONE',  ( -13.83973345681288158, 3.969039569021246550, 5.242263935944164288 ) ) ;
#9618 = CARTESIAN_POINT ( 'NONE',  ( 8.027808582316792396, -23.72900456129165647, 4.275561207030568411 ) ) ;
#9619 = CARTESIAN_POINT ( 'NONE',  ( -12.62500028073152869, -20.99998582305707728, 4.544498183892649479 ) ) ;
#9620 = FACE_OUTER_BOUND ( 'NONE', #8579, .T. ) ;
#9621 = CARTESIAN_POINT ( 'NONE',  ( -7.934058582316796837, -23.73192549717337130, 5.303608408759367343 ) ) ;
#9622 = CARTESIAN_POINT ( 'NONE',  ( 8.309058582316792396, -23.27327832286945153, 2.298404588716537411 ) ) ;
#9623 = CARTESIAN_POINT ( 'NONE',  ( 6.534691417683177406, -20.97900456129164581, 3.136473910504570917 ) ) ;
#9624 = CARTESIAN_POINT ( 'NONE',  ( -7.659691417683176518, -22.67418626127524917, 1.729004561291651587 ) ) ;
#9625 = VECTOR ( 'NONE', #5407, 1000.000000000000000 ) ;
#9626 = VERTEX_POINT ( 'NONE', #5917 ) ;
#9627 = EDGE_LOOP ( 'NONE', ( #1951, #6017, #18212, #12993 ) ) ;
#9628 = CARTESIAN_POINT ( 'NONE',  ( 13.37500000000002132, -20.24999999999450040, 3.833333333368183382 ) ) ;
#9629 = VECTOR ( 'NONE', #8563, 1000.000000000000000 ) ;
#9630 = CARTESIAN_POINT ( 'NONE',  ( 30.00000000000000000, 0.000000000000000000, 1.000000000000000000 ) ) ;
#9631 = VERTEX_POINT ( 'NONE', #7282 ) ;
#9632 = AXIS2_PLACEMENT_3D ( 'NONE', #17532, #74, #3211 ) ;
#9633 = EDGE_CURVE ( 'NONE', #3395, #4592, #16996, .T. ) ;
#9634 = VERTEX_POINT ( 'NONE', #7392 ) ;
#9635 = DIRECTION ( 'NONE',  ( 1.000000000000000000, 0.000000000000000000, 0.000000000000000000 ) ) ;
#9636 = CARTESIAN_POINT ( 'NONE',  ( 11.00000000000000000, -23.70993649053891517, 5.466506350946108483 ) ) ;
#9637 = CARTESIAN_POINT ( 'NONE',  ( -13.12529397354238192, 5.014845663890295846, 4.791666666666685614 ) ) ;
#9638 = VECTOR ( 'NONE', #11748, 1000.000000000000000 ) ;
#9639 = CARTESIAN_POINT ( 'NONE',  ( -0.5631383031621635116, -9.114917468222230923, 2.372643865078341019 ) ) ;
#9640 = CARTESIAN_POINT ( 'NONE',  ( -15.49999999999998224, -17.49999999999999645, 4.000000000000000000 ) ) ;
#9641 = VECTOR ( 'NONE', #7164, 1000.000000000000000 ) ;
#9642 = CARTESIAN_POINT ( 'NONE',  ( 2.693754455098655409, -10.04853567022903782, 2.237415670251142519 ) ) ;
#9643 = CARTESIAN_POINT ( 'NONE',  ( -12.64511805349267526, -19.23403829861753422, 5.507852591554869726 ) ) ;
#9644 = LINE ( 'NONE', #12782, #15099 ) ;
#9645 = CARTESIAN_POINT ( 'NONE',  ( -3.999999999999999112, -2.500000000000047518, 2.000000000000000000 ) ) ;
#9646 = CARTESIAN_POINT ( 'NONE',  ( 13.15047398821051239, 5.536436404627260721, 5.896317606305554015 ) ) ;
#9647 = AXIS2_PLACEMENT_3D ( 'NONE', #15648, #4568, #1335 ) ;
#9648 = EDGE_CURVE ( 'NONE', #12998, #13229, #1001, .T. ) ;
#9649 = CARTESIAN_POINT ( 'NONE',  ( -2.167793999318431197, -10.98794063836983703, 1.911058649813994315 ) ) ;
#9650 = VERTEX_POINT ( 'NONE', #11977 ) ;
#9651 = CARTESIAN_POINT ( 'NONE',  ( -13.87470602645761986, 4.985154336109792972, 4.166666666666765551 ) ) ;
#9652 = DIRECTION ( 'NONE',  ( 0.000000000000000000, 1.000000000000000000, 0.000000000000000000 ) ) ;
#9653 = CARTESIAN_POINT ( 'NONE',  ( 8.128441417683177406, -19.49999999999998934, 3.550687472877664952 ) ) ;
#9654 = CARTESIAN_POINT ( 'NONE',  ( -8.777808582316797725, -21.02099543870833998, 3.035098964749253003 ) ) ;
#9655 = EDGE_LOOP ( 'NONE', ( #2328, #18050, #2947, #18939 ) ) ;
#9656 = VECTOR ( 'NONE', #12929, 1000.000000000000000 ) ;
#9657 = CARTESIAN_POINT ( 'NONE',  ( 13.85716935893578317, 3.349552626256921517, 6.729005269197402939 ) ) ;
#9658 = CARTESIAN_POINT ( 'NONE',  ( 12.69247507894198712, -16.84250851341299082, 5.559274842915185033 ) ) ;
#9659 = AXIS2_PLACEMENT_3D ( 'NONE', #7999, #6540, #16055 ) ;
#9660 = CARTESIAN_POINT ( 'NONE',  ( -3.500698171653725765, 0.000000000000000000, 0.000000000000000000 ) ) ;
#9661 = ORIENTED_EDGE ( 'NONE', *, *, #11698, .F. ) ;
#9662 = EDGE_CURVE ( 'NONE', #4337, #17093, #20384, .T. ) ;
#9663 = CIRCLE ( 'NONE', #15328, 2.500000000000000444 ) ;
#9664 = EDGE_LOOP ( 'NONE', ( #2778, #16242, #12393, #15833 ) ) ;
#9665 = EDGE_CURVE ( 'NONE', #18399, #9362, #12288, .T. ) ;
#9666 = DIRECTION ( 'NONE',  ( 0.000000000000000000, 0.000000000000000000, 1.000000000000000000 ) ) ;
#9667 = CARTESIAN_POINT ( 'NONE',  ( 19.19064177244175440, 11.64110105645932691, 0.000000000000000000 ) ) ;
#9668 = CARTESIAN_POINT ( 'NONE',  ( -14.49999999999998579, -19.49999999999999645, 1.000000000000000000 ) ) ;
#9669 = LINE ( 'NONE', #3287, #8661 ) ;
#9670 = CARTESIAN_POINT ( 'NONE',  ( 2.044552395631970665, -10.13052631352519306, 1.690857522621936226 ) ) ;
#9671 = PLANE ( 'NONE',  #8198 ) ;
#9672 = FACE_OUTER_BOUND ( 'NONE', #2981, .T. ) ;
#9673 = EDGE_CURVE ( 'NONE', #19645, #18629, #18682, .T. ) ;
#9674 = CARTESIAN_POINT ( 'NONE',  ( -27.52582389412042474, 4.853545418763153485, 0.000000000000000000 ) ) ;
#9675 = DIRECTION ( 'NONE',  ( -0.000000000000000000, -0.000000000000000000, -1.000000000000000000 ) ) ;
#9676 = CARTESIAN_POINT ( 'NONE',  ( 5.683390479346035029, 0.000000000000000000, 1.000000000000000000 ) ) ;
#9677 = CARTESIAN_POINT ( 'NONE',  ( 0.3749999999999968914, 4.999999999999999112, 1.000000000000000000 ) ) ;
#9678 = CIRCLE ( 'NONE', #659, 1.499999999999998668 ) ;
#9679 = CARTESIAN_POINT ( 'NONE',  ( 8.965308582316795949, -20.97900456129165647, 3.863526089495444626 ) ) ;
#9680 = CARTESIAN_POINT ( 'NONE',  ( -12.63298722613685676, -19.09664508008815531, 4.760766981674283471 ) ) ;
#9681 = CARTESIAN_POINT ( 'NONE',  ( -11.40280858231679417, -22.77556120703056308, 1.770995438708339975 ) ) ;
#9682 = AXIS2_PLACEMENT_3D ( 'NONE', #516, #1982, #19664 ) ;
#9683 = CARTESIAN_POINT ( 'NONE',  ( -10.65969141768318096, -22.67418626127524917, 1.729004561291651809 ) ) ;
#9684 = EDGE_LOOP ( 'NONE', ( #8161, #13691, #715, #5181 ) ) ;
#9685 = CARTESIAN_POINT ( 'NONE',  ( 13.84074239313819277, 4.019990853478630832, 5.241358430878110930 ) ) ;
#9686 = LINE ( 'NONE', #5086, #13716 ) ;
#9687 = ORIENTED_EDGE ( 'NONE', *, *, #1313, .T. ) ;
#9688 = VERTEX_POINT ( 'NONE', #4349 ) ;
#9689 = CARTESIAN_POINT ( 'NONE',  ( 0.000000000000000000, 4.999999999999999112, 1.000000000000000000 ) ) ;
#9690 = ORIENTED_EDGE ( 'NONE', *, *, #19019, .T. ) ;
#9691 = FACE_OUTER_BOUND ( 'NONE', #3728, .T. ) ;
#9692 = VECTOR ( 'NONE', #18791, 1000.000000000000000 ) ;
#9693 = VECTOR ( 'NONE', #434, 1000.000000000000000 ) ;
#9694 = VERTEX_POINT ( 'NONE', #19850 ) ;
#9695 = CARTESIAN_POINT ( 'NONE',  ( 12.15969141768317563, -22.67418626127524917, 1.729004561291651587 ) ) ;
#9696 = CARTESIAN_POINT ( 'NONE',  ( 26.69203811574920238, 10.00000000000000000, 1.000000000000000000 ) ) ;
#9697 = VECTOR ( 'NONE', #17835, 1000.000000000000000 ) ;
#9698 = CARTESIAN_POINT ( 'NONE',  ( -0.9854920305337621089, -9.114917468222230923, 2.372643865078341019 ) ) ;
#9699 = CARTESIAN_POINT ( 'NONE',  ( -0.000000000000000000, 11.64110105645932691, 0.000000000000000000 ) ) ;
#9700 = CARTESIAN_POINT ( 'NONE',  ( -10.37155858231679417, -20.24999999999999289, 3.449312527122348371 ) ) ;
#9701 = ADVANCED_FACE ( 'NONE', ( #2785, #10733 ), #9161, .F. ) ;
#9702 = CARTESIAN_POINT ( 'NONE',  ( 8.876396343307449754, 0.000000000000000000, 1.000000000000000000 ) ) ;
#9703 = CARTESIAN_POINT ( 'NONE',  ( 6.628441417683176518, -20.24999999999999289, 3.550687472877664952 ) ) ;
#9704 = CYLINDRICAL_SURFACE ( 'NONE', #16885, 0.2500000000000002220 ) ;
#9705 = CARTESIAN_POINT ( 'NONE',  ( -6.065941417683177406, -23.20159541128344927, 2.226721677130534705 ) ) ;
#9706 = ORIENTED_EDGE ( 'NONE', *, *, #9606, .F. ) ;
#9707 = CARTESIAN_POINT ( 'NONE',  ( 7.184058582316795949, -20.26807450282662160, 1.696391591240633101 ) ) ;
#9708 = DIRECTION ( 'NONE',  ( -0.000000000000000000, -0.000000000000000000, -1.000000000000000000 ) ) ;
#9709 = CARTESIAN_POINT ( 'NONE',  ( -12.64802275499843454, -19.83735087257960927, 6.157588447769994922 ) ) ;
#9710 = ORIENTED_EDGE ( 'NONE', *, *, #16136, .F. ) ;
#9711 = AXIS2_PLACEMENT_3D ( 'NONE', #16984, #20147, #7070 ) ;
#9712 = VECTOR ( 'NONE', #5078, 1000.000000000000000 ) ;
#9713 = PLANE ( 'NONE',  #18647 ) ;
#9714 = LINE ( 'NONE', #1768, #5992 ) ;
#9715 = AXIS2_PLACEMENT_3D ( 'NONE', #16887, #8848, #18570 ) ;
#9716 = ORIENTED_EDGE ( 'NONE', *, *, #1059, .F. ) ;
#9717 = CARTESIAN_POINT ( 'NONE',  ( 0.000000000000000000, 0.000000000000000000, 0.000000000000000000 ) ) ;
#9718 = ORIENTED_EDGE ( 'NONE', *, *, #7952, .F. ) ;
#9719 = DIRECTION ( 'NONE',  ( 1.000000000000000000, 0.000000000000000000, 0.000000000000000000 ) ) ;
#9720 = ORIENTED_EDGE ( 'NONE', *, *, #15355, .F. ) ;
#9721 = CARTESIAN_POINT ( 'NONE',  ( -11.87155858231679595, -19.49999999999998934, 3.449312527122348371 ) ) ;
#9722 = CARTESIAN_POINT ( 'NONE',  ( 12.62745083560477966, -20.12623280195927933, 5.001038150054709419 ) ) ;
#9723 = PLANE ( 'NONE',  #12790 ) ;
#9724 = CARTESIAN_POINT ( 'NONE',  ( 1.897597015127918230, -9.924601616748528699, 1.637971946730535588 ) ) ;
#9725 = VECTOR ( 'NONE', #7034, 1000.000000000000000 ) ;
#9726 = CARTESIAN_POINT ( 'NONE',  ( 13.02818618459764188, 0.1109023222084986743, 5.923858176248589125 ) ) ;
#9727 = VECTOR ( 'NONE', #2621, 1000.000000000000000 ) ;
#9728 = CARTESIAN_POINT ( 'NONE',  ( -13.49999999999998401, -21.99999999999999645, 14.18378559369222280 ) ) ;
#9729 = CARTESIAN_POINT ( 'NONE',  ( -13.76337198624852398, 0.1127853055781036368, 5.159333296715827188 ) ) ;
#9730 = CARTESIAN_POINT ( 'NONE',  ( 10.93405858231679595, -23.73192549717337130, 5.303608408759367343 ) ) ;
#9731 = CARTESIAN_POINT ( 'NONE',  ( -13.08107971211413378, 2.032025461757085427, 6.715204579155630960 ) ) ;
#9732 = ADVANCED_FACE ( 'NONE', ( #10524 ), #800, .T. ) ;
#9733 = DIRECTION ( 'NONE',  ( 1.000000000000000000, 0.000000000000000000, 0.000000000000000000 ) ) ;
#9734 = CARTESIAN_POINT ( 'NONE',  ( 5.777808582316794173, -20.27099543870833642, 2.724438792969431589 ) ) ;
#9735 = CARTESIAN_POINT ( 'NONE',  ( 8.690941417683177406, -22.74294823697955081, 4.171265325393542334 ) ) ;
#9736 = CARTESIAN_POINT ( 'NONE',  ( -5.315941417683176518, -20.79840458871654363, 4.773278322869464851 ) ) ;
#9737 = ORIENTED_EDGE ( 'NONE', *, *, #1060, .F. ) ;
#9738 = EDGE_LOOP ( 'NONE', ( #20299, #17688, #4798, #10770 ) ) ;
#9739 = EDGE_CURVE ( 'NONE', #15705, #6243, #8753, .T. ) ;
#9740 = CARTESIAN_POINT ( 'NONE',  ( 13.84501469867711698, 4.235742283194553259, 4.916666666666649199 ) ) ;
#9741 = EDGE_CURVE ( 'NONE', #7048, #10510, #15321, .T. ) ;
#9742 = FACE_OUTER_BOUND ( 'NONE', #15033, .T. ) ;
#9743 = DIRECTION ( 'NONE',  ( -0.000000000000000000, -0.000000000000000000, -1.000000000000000000 ) ) ;
#9744 = ORIENTED_EDGE ( 'NONE', *, *, #18430, .F. ) ;
#9745 = AXIS2_PLACEMENT_3D ( 'NONE', #1151, #8890, #10772 ) ;
#9746 = EDGE_LOOP ( 'NONE', ( #2383, #2976, #20352, #20277, #18412, #1155 ) ) ;
#9747 = DIRECTION ( 'NONE',  ( -0.000000000000000000, -0.000000000000000000, -1.000000000000000000 ) ) ;
#9748 = FACE_OUTER_BOUND ( 'NONE', #12154, .T. ) ;
#9749 = CARTESIAN_POINT ( 'NONE',  ( 10.38119784648305810, -14.00000000000000000, 2.000000000000000000 ) ) ;
#9750 = CARTESIAN_POINT ( 'NONE',  ( -2.532303758294933704, -8.551221675625164664, 1.670490507339845054 ) ) ;
#9751 = FACE_OUTER_BOUND ( 'NONE', #4157, .T. ) ;
#9752 = DIRECTION ( 'NONE',  ( 1.000000000000000000, 0.000000000000000000, -0.000000000000000000 ) ) ;
#9753 = CARTESIAN_POINT ( 'NONE',  ( -12.62499979224180180, -20.25001049178813162, 4.458178821399696012 ) ) ;
#9754 = CARTESIAN_POINT ( 'NONE',  ( 11.21530858231679417, -23.77099543870833998, 2.825813738724734847 ) ) ;
#9755 = FACE_OUTER_BOUND ( 'NONE', #13578, .T. ) ;
#9756 = CARTESIAN_POINT ( 'NONE',  ( 13.15498530132288479, 5.764257716805535559, 4.583333333333295734 ) ) ;
#9757 = CIRCLE ( 'NONE', #745, 59.99999999999998579 ) ;
#9758 = ADVANCED_FACE ( 'NONE', ( #18377 ), #16794, .T. ) ;
#9759 = CARTESIAN_POINT ( 'NONE',  ( -2.442511739767545098, -14.09457879449248807, 3.458905389639174821 ) ) ;
#9760 = ORIENTED_EDGE ( 'NONE', *, *, #3902, .T. ) ;
#9761 = CARTESIAN_POINT ( 'NONE',  ( -13.37500000000002132, -20.99999999999450395, 3.833333333368183382 ) ) ;
#9762 = CARTESIAN_POINT ( 'NONE',  ( 17.30017143803810242, 9.000000000000001776, 1.000000000000000000 ) ) ;
#9763 = CARTESIAN_POINT ( 'NONE',  ( 4.753441417683176518, -21.94931252712233061, 0.9999999999999978906 ) ) ;
#9764 = CARTESIAN_POINT ( 'NONE',  ( -6.715308582316796837, -23.02099543870833998, 3.136473910504556262 ) ) ;
#9765 = ORIENTED_EDGE ( 'NONE', *, *, #8851, .T. ) ;
#9766 = CARTESIAN_POINT ( 'NONE',  ( 13.67732412376249052, -5.732631749971324631, 6.533692769198849781 ) ) ;
#9767 = CARTESIAN_POINT ( 'NONE',  ( 13.12529397354238192, 5.014845663890295846, 4.333333333333382775 ) ) ;
#9768 = PLANE ( 'NONE',  #14339 ) ;
#9769 = AXIS2_PLACEMENT_3D ( 'NONE', #17199, #16228, #9841 ) ;
#9770 = VERTEX_POINT ( 'NONE', #15221 ) ;
#9771 = ORIENTED_EDGE ( 'NONE', *, *, #5397, .T. ) ;
#9772 = DIRECTION ( 'NONE',  ( 1.000000000000000000, 0.000000000000000000, 0.000000000000000000 ) ) ;
#9773 = VECTOR ( 'NONE', #10393, 1000.000000000000000 ) ;
#9774 = DIRECTION ( 'NONE',  ( 1.000000000000000000, 0.000000000000000000, 0.000000000000000000 ) ) ;
#9775 = ORIENTED_EDGE ( 'NONE', *, *, #9284, .F. ) ;
#9776 = DIRECTION ( 'NONE',  ( 0.000000000000000000, -0.000000000000000000, 1.000000000000000000 ) ) ;
#9777 = CARTESIAN_POINT ( 'NONE',  ( 1.744064896197293324, -9.868721669903177229, 1.623620860066563365 ) ) ;
#9778 = DIRECTION ( 'NONE',  ( -1.000000000000000000, 0.000000000000000000, 0.000000000000000000 ) ) ;
#9779 = CARTESIAN_POINT ( 'NONE',  ( 10.18924542913430820, 11.64110105645932691, 10.00000000000000000 ) ) ;
#9780 = ADVANCED_FACE ( 'NONE', ( #5717 ), #4140, .T. ) ;
#9781 = LINE ( 'NONE', #8116, #7 ) ;
#9782 = LINE ( 'NONE', #19110, #8977 ) ;
#9783 = CARTESIAN_POINT ( 'NONE',  ( -11.02780858231679595, -23.72900456129165647, 4.275561207030568411 ) ) ;
#9784 = EDGE_CURVE ( 'NONE', #12628, #4517, #18320, .T. ) ;
#9785 = CARTESIAN_POINT ( 'NONE',  ( -2.436080212393455735, -9.483920418190111334, 2.467411194204634839 ) ) ;
#9786 = EDGE_LOOP ( 'NONE', ( #532, #9257 ) ) ;
#9787 = CARTESIAN_POINT ( 'NONE',  ( -13.09543520949579865, 4.256978079540234106, 5.067654010725516578 ) ) ;
#9788 = CARTESIAN_POINT ( 'NONE',  ( -11.12155858231679417, -23.74999999999999645, 3.550687472877651629 ) ) ;
#9789 = AXIS2_PLACEMENT_3D ( 'NONE', #5765, #11922, #5866 ) ;
#9790 = CARTESIAN_POINT ( 'NONE',  ( -4.753441417683176518, -21.94931252712233061, 1.749999999999998446 ) ) ;
#9791 = ORIENTED_EDGE ( 'NONE', *, *, #20680, .F. ) ;
#9792 = CARTESIAN_POINT ( 'NONE',  ( 13.41806913471718588, -17.32500869677464550, 4.784333296715663764 ) ) ;
#9793 = ORIENTED_EDGE ( 'NONE', *, *, #19128, .T. ) ;
#9794 = EDGE_LOOP ( 'NONE', ( #19428, #1862, #12635, #9129, #6769 ) ) ;
#9795 = DIRECTION ( 'NONE',  ( 0.000000000000000000, 0.000000000000000000, 1.000000000000000000 ) ) ;
#9796 = ORIENTED_EDGE ( 'NONE', *, *, #18506, .F. ) ;
#9797 = LINE ( 'NONE', #176, #1747 ) ;
#9798 = EDGE_CURVE ( 'NONE', #14709, #13635, #17509, .T. ) ;
#9799 = B_SPLINE_CURVE_WITH_KNOTS ( 'NONE', 3,
 ( #15702, #1278, #4519, #4612, #17375, #13921, #12464, #4827, #7658, #10804, #9434, #11005, #1386, #20634, #20322, #17173, #15595, #6190, #2850, #3060, #15807, #10905, #14132, #12558, #20537, #1484, #5985, #14028, #18959, #19063 ),
 .UNSPECIFIED., .F., .F.,
 ( 4, 2, 2, 2, 2, 2, 2, 2, 2, 2, 2, 2, 2, 2, 4 ),
 ( 0.6080100341812841869, 0.6200887121040892236, 0.6309950902025724950, 0.6419014683010558775, 0.6637142244980225314, 0.7073397368919559502, 0.7509652492858893691, 0.7727780054828560230, 0.7836843835813394055, 0.7945907616798226769, 0.8074288390748337596, 0.8202669164698448423, 0.8459430712598670077, 0.8972953808399113385, 1.000000000000000000 ),
 .UNSPECIFIED. ) ;
#9800 = ORIENTED_EDGE ( 'NONE', *, *, #15724, .T. ) ;
#9801 = CARTESIAN_POINT ( 'NONE',  ( 10.09719141768317563, -22.77556120703057729, 5.229004561291656472 ) ) ;
#9802 = CARTESIAN_POINT ( 'NONE',  ( -13.17791111847408025, 9.000000000000001776, 1.000000000000000000 ) ) ;
#9803 = CARTESIAN_POINT ( 'NONE',  ( -1.337453470010121714, -9.864917468222230923, 2.372643865078341019 ) ) ;
#9804 = CARTESIAN_POINT ( 'NONE',  ( -10.43924542913431175, 11.64110105645932691, 10.00000000000000000 ) ) ;
#9805 = CARTESIAN_POINT ( 'NONE',  ( -9.809058582316794173, -23.27327832286945153, 2.298404588716537411 ) ) ;
#9806 = CARTESIAN_POINT ( 'NONE',  ( -7.626396343307448866, 10.00000000000000000, 1.000000000000000000 ) ) ;
#9807 = CARTESIAN_POINT ( 'NONE',  ( 8.315941417683177406, -20.79840458871654363, 4.773278322869464851 ) ) ;
#9808 = DIRECTION ( 'NONE',  ( -0.000000000000000000, 0.000000000000000000, -1.000000000000000000 ) ) ;
#9809 = CARTESIAN_POINT ( 'NONE',  ( -12.25344141768317741, -21.94931252712233061, 2.499999999999999112 ) ) ;
#9810 = VECTOR ( 'NONE', #5449, 1000.000000000000000 ) ;
#9811 = ORIENTED_EDGE ( 'NONE', *, *, #16297, .F. ) ;
#9812 = CARTESIAN_POINT ( 'NONE',  ( 10.93405858231679595, -23.73192549717337130, 5.303608408759367343 ) ) ;
#9813 = CARTESIAN_POINT ( 'NONE',  ( 12.72125031657057015, -15.38935901321805133, 5.590524842915047365 ) ) ;
#9814 = CARTESIAN_POINT ( 'NONE',  ( -13.11644927503132330, 3.818188389080370282, 6.753616037489316604 ) ) ;
#9815 = ORIENTED_EDGE ( 'NONE', *, *, #16308, .F. ) ;
#9816 = LINE ( 'NONE', #13156, #16959 ) ;
#9817 = DIRECTION ( 'NONE',  ( 0.000000000000000000, 1.000000000000000000, -0.000000000000000000 ) ) ;
#9818 = ORIENTED_EDGE ( 'NONE', *, *, #12618, .T. ) ;
#9819 = DIRECTION ( 'NONE',  ( 1.000000000000000000, 0.000000000000000000, 0.000000000000000000 ) ) ;
#9820 = ORIENTED_EDGE ( 'NONE', *, *, #13005, .F. ) ;
#9821 = EDGE_CURVE ( 'NONE', #10023, #12236, #3191, .T. ) ;
#9822 = CARTESIAN_POINT ( 'NONE',  ( 12.69874195915161330, -20.02071431810549740, 3.541097010573131421 ) ) ;
#9823 = ORIENTED_EDGE ( 'NONE', *, *, #1570, .F. ) ;
#9824 = CARTESIAN_POINT ( 'NONE',  ( -4.934058582316793284, -23.20159541128345992, 4.773278322869455970 ) ) ;
#9825 = CARTESIAN_POINT ( 'NONE',  ( 13.09532840572934376, 3.501584489333809724, 5.996774842915142401 ) ) ;
#9826 = CARTESIAN_POINT ( 'NONE',  ( 0.000000000000000000, 0.000000000000000000, 4.000000000000000000 ) ) ;
#9827 = CARTESIAN_POINT ( 'NONE',  ( 12.62499999999998224, -20.24999999999998934, 4.166666666666636765 ) ) ;
#9828 = PRODUCT_DEFINITION ( 'UNKNOWN', '', #10035, #7961 ) ;
#9829 = FACE_OUTER_BOUND ( 'NONE', #18882, .T. ) ;
#9830 = CARTESIAN_POINT ( 'NONE',  ( -13.84439157666246878, 4.204274621457510186, 5.123803251657143676 ) ) ;
#9831 = CARTESIAN_POINT ( 'NONE',  ( 8.215308582316795949, -24.52099543870834708, 2.515153566944913432 ) ) ;
#9832 = CARTESIAN_POINT ( 'NONE',  ( -12.81251082758882376, -11.53070320674076576, 6.423537912489145185 ) ) ;
#9833 = CARTESIAN_POINT ( 'NONE',  ( -11.03469141768317741, -19.47900456129164581, 2.515153566944927199 ) ) ;
#9834 = DIRECTION ( 'NONE',  ( 1.000000000000000000, 0.000000000000000000, 0.000000000000000000 ) ) ;
#9835 = DIRECTION ( 'NONE',  ( -0.000000000000000000, -0.000000000000000000, -1.000000000000000000 ) ) ;
#9836 = CARTESIAN_POINT ( 'NONE',  ( 7.652808582316796837, -21.53509896474924901, 4.479004561291659137 ) ) ;
#9837 = CARTESIAN_POINT ( 'NONE',  ( -5.034691417683179182, -20.22900456129164581, 2.825813738724748170 ) ) ;
#9838 = VERTEX_POINT ( 'NONE', #20571 ) ;
#9839 = ORIENTED_EDGE ( 'NONE', *, *, #12578, .F. ) ;
#9840 = CARTESIAN_POINT ( 'NONE',  ( 13.84501465882535598, 4.235740270674679842, 5.020612255068622076 ) ) ;
#9841 = DIRECTION ( 'NONE',  ( 0.000000000000000000, 0.000000000000000000, 1.000000000000000000 ) ) ;
#9842 =( NAMED_UNIT ( * ) SI_UNIT ( $, .STERADIAN. ) SOLID_ANGLE_UNIT ( ) );
#9843 = ORIENTED_EDGE ( 'NONE', *, *, #7331, .T. ) ;
#9844 = VERTEX_POINT ( 'NONE', #1317 ) ;
#9845 = LINE ( 'NONE', #13279, #11118 ) ;
#9846 = DIRECTION ( 'NONE',  ( 1.000000000000000000, 0.000000000000000000, 0.000000000000000000 ) ) ;
#9847 = EDGE_CURVE ( 'NONE', #17893, #16449, #1420, .T. ) ;
#9848 = CARTESIAN_POINT ( 'NONE',  ( -13.12529397354238192, 5.014845663890295846, 4.166666666666749563 ) ) ;
#9849 = LINE ( 'NONE', #4647, #19892 ) ;
#9850 = DIRECTION ( 'NONE',  ( -0.000000000000000000, -0.000000000000000000, -1.000000000000000000 ) ) ;
#9851 = VECTOR ( 'NONE', #13500, 1000.000000000000000 ) ;
#9852 = CARTESIAN_POINT ( 'NONE',  ( -13.05696142222617695, 1.564051822406025583, 5.955108176248398166 ) ) ;
#9853 = CARTESIAN_POINT ( 'NONE',  ( 4.687312169500630787, -21.51559725698340131, 5.182386163300424009 ) ) ;
#9854 = CARTESIAN_POINT ( 'NONE',  ( 0.000000000000000000, 11.64110105645932691, 10.00000000000000000 ) ) ;
#9855 = CARTESIAN_POINT ( 'NONE',  ( 13.12270769621861355, 4.884238659038159902, 5.513847264053151065 ) ) ;
#9856 = CARTESIAN_POINT ( 'NONE',  ( -1.407845757905374695, -9.114917468222230923, 2.372643865078341019 ) ) ;
#9857 = EDGE_LOOP ( 'NONE', ( #18187, #14305, #9125, #15104 ) ) ;
#9858 = CARTESIAN_POINT ( 'NONE',  ( -13.81626551376501588, 2.033908445126689557, 5.950679699622869911 ) ) ;
#9859 = LINE ( 'NONE', #1713, #2037 ) ;
#9860 = VECTOR ( 'NONE', #13759, 1000.000000000000000 ) ;
#9861 = CARTESIAN_POINT ( 'NONE',  ( 4.284691417683177406, -24.52099543870834708, 4.484846433055073689 ) ) ;
#9862 = CARTESIAN_POINT ( 'NONE',  ( -9.527808582316795949, -22.97900456129165647, 3.964901035250747885 ) ) ;
#9863 = EDGE_LOOP ( 'NONE', ( #8510, #14195, #14703, #19082 ) ) ;
#9864 = CARTESIAN_POINT ( 'NONE',  ( 12.62499999999998401, -20.99999999999999645, 3.146526952850934755 ) ) ;
#9865 = CARTESIAN_POINT ( 'NONE',  ( 13.12463908936614132, 4.981774012991869505, 5.264611377988129171 ) ) ;
#9866 = PLANE ( 'NONE',  #11668 ) ;
#9867 = ORIENTED_EDGE ( 'NONE', *, *, #13582, .T. ) ;
#9868 = ORIENTED_EDGE ( 'NONE', *, *, #19526, .T. ) ;
#9869 = CARTESIAN_POINT ( 'NONE',  ( -4.999999999999998224, -7.500000000000047073, 9.999999999999998224 ) ) ;
#9870 = AXIS2_PLACEMENT_3D ( 'NONE', #14193, #20600, #19138 ) ;
#9871 = EDGE_CURVE ( 'NONE', #19457, #2445, #1215, .T. ) ;
#9872 = PLANE ( 'NONE',  #1554 ) ;
#9873 = FACE_OUTER_BOUND ( 'NONE', #9857, .T. ) ;
#9874 = EDGE_CURVE ( 'NONE', #17197, #9600, #53, .T. ) ;
#9875 = CARTESIAN_POINT ( 'NONE',  ( -0.000000000000000000, 10.00000000000000000, 0.000000000000000000 ) ) ;
#9876 = CARTESIAN_POINT ( 'NONE',  ( 1.882415164465650825, -10.11790622164856224, 2.437616430916333510 ) ) ;
#9877 = DIRECTION ( 'NONE',  ( 0.000000000000000000, 0.000000000000000000, 1.000000000000000000 ) ) ;
#9878 = EDGE_CURVE ( 'NONE', #5573, #15088, #20667, .T. ) ;
#9879 = CARTESIAN_POINT ( 'NONE',  ( 0.000000000000000000, 0.000000000000000000, 1.000000000000000000 ) ) ;
#9880 = CARTESIAN_POINT ( 'NONE',  ( 16.37779268661489596, 11.64110105645932691, 0.000000000000000000 ) ) ;
#9881 = LINE ( 'NONE', #1832, #19009 ) ;
#9882 = CARTESIAN_POINT ( 'NONE',  ( -11.74178095869206828, 0.000000000000000000, 1.000000000000000000 ) ) ;
#9883 = CARTESIAN_POINT ( 'NONE',  ( -3.317048600639548095, -9.800042196285016161, 2.741212564741740465 ) ) ;
#9884 = ORIENTED_EDGE ( 'NONE', *, *, #1439, .F. ) ;
#9885 = VECTOR ( 'NONE', #6569, 1000.000000000000000 ) ;
#9886 = CARTESIAN_POINT ( 'NONE',  ( -12.82182472306881671, -9.560351485048736109, 4.965845106672846399 ) ) ;
#9887 = EDGE_CURVE ( 'NONE', #8074, #20271, #7897, .T. ) ;
#9888 = CARTESIAN_POINT ( 'NONE',  ( -4.687312169500634340, -21.70215802671379990, 4.455959925339818106 ) ) ;
#9889 = CARTESIAN_POINT ( 'NONE',  ( -8.972191417683177406, -23.72900456129165292, 2.724438792969417822 ) ) ;
#9890 = VERTEX_POINT ( 'NONE', #3093 ) ;
#9891 = CARTESIAN_POINT ( 'NONE',  ( 13.84501469867711698, 4.235742283194553259, 4.833333333333343695 ) ) ;
#9892 =( NAMED_UNIT ( * ) SI_UNIT ( $, .STERADIAN. ) SOLID_ANGLE_UNIT ( ) );
#9893 = ORIENTED_EDGE ( 'NONE', *, *, #2951, .F. ) ;
#9894 = VERTEX_POINT ( 'NONE', #6223 ) ;
#9895 = CARTESIAN_POINT ( 'NONE',  ( -4.000000000000000000, -8.500000000000000000, 2.392927049865408495 ) ) ;
#9896 = ORIENTED_EDGE ( 'NONE', *, *, #10991, .F. ) ;
#9897 = PLANE ( 'NONE',  #4086 ) ;
#9898 = EDGE_CURVE ( 'NONE', #7416, #3395, #17303, .T. ) ;
#9899 = VERTEX_POINT ( 'NONE', #15530 ) ;
#9900 = LINE ( 'NONE', #19849, #6997 ) ;
#9901 = CARTESIAN_POINT ( 'NONE',  ( -9.000000000000000000, -9.999999999999992895, 2.500000000000000000 ) ) ;
#9902 = CARTESIAN_POINT ( 'NONE',  ( -2.559937518207947793, -9.746075135043517079, 2.534737762559237773 ) ) ;
#9903 = DIRECTION ( 'NONE',  ( -1.000000000000000000, 0.000000000000000000, 0.000000000000000000 ) ) ;
#9904 = CARTESIAN_POINT ( 'NONE',  ( -9.059058582316794173, -20.72672167713054137, 4.701595411283463477 ) ) ;
#9905 = DIRECTION ( 'NONE',  ( -1.000000000000000000, 0.000000000000000000, 0.000000000000000000 ) ) ;
#9906 = CARTESIAN_POINT ( 'NONE',  ( 9.909691417683179182, -21.32581373872474373, 5.270995438708348857 ) ) ;
#9907 = PLANE ( 'NONE',  #9538 ) ;
#9908 = ADVANCED_FACE ( 'NONE', ( #7802 ), #13956, .T. ) ;
#9909 = CARTESIAN_POINT ( 'NONE',  ( -4.378441417683176518, -23.74999999999999645, 3.449312527122335492 ) ) ;
#9910 = VERTEX_POINT ( 'NONE', #6439 ) ;
#9911 = CARTESIAN_POINT ( 'NONE',  ( 12.24655858231679595, -21.94931252712234127, 6.000000000000001776 ) ) ;
#9912 = CARTESIAN_POINT ( 'NONE',  ( 13.02818618459764188, 0.1109023222084986743, 5.923858176248589125 ) ) ;
#9913 = CARTESIAN_POINT ( 'NONE',  ( -12.63819864697926754, -19.58346832754827105, 5.450273968536036406 ) ) ;
#9914 = EDGE_LOOP ( 'NONE', ( #9101, #1845 ) ) ;
#9915 = VECTOR ( 'NONE', #7255, 1000.000000000000000 ) ;
#9916 = FACE_OUTER_BOUND ( 'NONE', #16701, .T. ) ;
#9917 = DIRECTION ( 'NONE',  ( 0.000000000000000000, -0.000000000000000000, 1.000000000000000000 ) ) ;
#9918 = ORIENTED_EDGE ( 'NONE', *, *, #13616, .F. ) ;
#9919 = ORIENTED_EDGE ( 'NONE', *, *, #20354, .F. ) ;
#9920 = ADVANCED_FACE ( 'NONE', ( #17205 ), #16961, .T. ) ;
#9921 = DIRECTION ( 'NONE',  ( -1.000000000000000000, -0.000000000000000000, 0.000000000000000000 ) ) ;
#9922 = EDGE_CURVE ( 'NONE', #10513, #11555, #17699, .T. ) ;
#9923 = ORIENTED_EDGE ( 'NONE', *, *, #1990, .F. ) ;
#9924 = DIRECTION ( 'NONE',  ( -0.000000000000000000, -0.000000000000000000, -1.000000000000000000 ) ) ;
#9925 = CARTESIAN_POINT ( 'NONE',  ( 14.31494360078803041, 16.00000000000000000, 1.000000000000000000 ) ) ;
#9926 = CARTESIAN_POINT ( 'NONE',  ( -3.999999999999999112, -7.500000000000047073, 2.000000000000000000 ) ) ;
#9927 = AXIS2_PLACEMENT_3D ( 'NONE', #1565, #1776, #19049 ) ;
#9928 = CARTESIAN_POINT ( 'NONE',  ( 12.68288333306630378, -17.32689168014509207, 5.548858176248425700 ) ) ;
#9929 = DIRECTION ( 'NONE',  ( 1.000000000000000000, 0.000000000000000000, 0.000000000000000000 ) ) ;
#9930 = CARTESIAN_POINT ( 'NONE',  ( -13.37499999999998224, -20.24999999999998934, 4.166666666666636765 ) ) ;
#9931 = AXIS2_PLACEMENT_3D ( 'NONE', #14108, #8052, #12847 ) ;
#9932 = CARTESIAN_POINT ( 'NONE',  ( 9.152808582316795949, -20.91377862118960351, 5.979004561291660913 ) ) ;
#9933 = CARTESIAN_POINT ( 'NONE',  ( -13.15498530132288479, 5.764257716805535559, 4.791666666666684726 ) ) ;
#9934 = EDGE_CURVE ( 'NONE', #13997, #193, #8566, .T. ) ;
#9935 = CARTESIAN_POINT ( 'NONE',  ( -5.496558582316795949, -22.05068747287764452, 0.9999999999999978906 ) ) ;
#9936 = CARTESIAN_POINT ( 'NONE',  ( 20.49999999999998224, -21.99999999999999645, 9.999999999999998224 ) ) ;
#9937 = LINE ( 'NONE', #1992, #11094 ) ;
#9938 = CARTESIAN_POINT ( 'NONE',  ( 11.59030858231679595, -21.63647391050454871, 2.479004561291657804 ) ) ;
#9939 = CARTESIAN_POINT ( 'NONE',  ( -6.440941417683176518, -20.72672167713052715, 2.298404588716546293 ) ) ;
#9940 = ORIENTED_EDGE ( 'NONE', *, *, #1874, .T. ) ;
#9941 = ORIENTED_EDGE ( 'NONE', *, *, #14525, .T. ) ;
#9942 = CARTESIAN_POINT ( 'NONE',  ( 13.84501469867711698, 4.235742283194553259, 3.666666666666500873 ) ) ;
#9943 = PLANE ( 'NONE',  #13429 ) ;
#9944 = SURFACE_STYLE_USAGE ( .BOTH. , #13082 ) ;
#9945 = ORIENTED_EDGE ( 'NONE', *, *, #7717, .F. ) ;
#9946 = LINE ( 'NONE', #19680, #8464 ) ;
#9947 = DIRECTION ( 'NONE',  ( 1.000000000000000000, 0.000000000000000000, 0.000000000000000000 ) ) ;
#9948 = CARTESIAN_POINT ( 'NONE',  ( 13.37500000000002132, -20.25000000000274269, 4.083333333315724012 ) ) ;
#9949 = DIRECTION ( 'NONE',  ( -0.000000000000000000, -0.000000000000000000, -1.000000000000000000 ) ) ;
#9950 = CARTESIAN_POINT ( 'NONE',  ( 3.211992482548209349, -9.366834950279640637, 2.629956289783360823 ) ) ;
#9951 = CARTESIAN_POINT ( 'NONE',  ( 1.513434189748285696, -9.114917468222230923, 1.622643865078341463 ) ) ;
#9952 = CARTESIAN_POINT ( 'NONE',  ( -13.08573665985359824, 3.017201322601628100, 5.986358176248492313 ) ) ;
#9953 = CARTESIAN_POINT ( 'NONE',  ( 5.027808582316793284, -23.72900456129165292, 4.275561207030568411 ) ) ;
#9954 = LINE ( 'NONE', #5462, #19103 ) ;
#9955 = CARTESIAN_POINT ( 'NONE',  ( 13.12529380813666435, 5.014837310896125722, 5.033295791462342628 ) ) ;
#9956 = EDGE_CURVE ( 'NONE', #16247, #7956, #6353, .T. ) ;
#9957 = VECTOR ( 'NONE', #16583, 1000.000000000000000 ) ;
#9958 = CARTESIAN_POINT ( 'NONE',  ( -1.337453470010121714, -9.114917468222230923, 2.372643865078341019 ) ) ;
#9959 = CARTESIAN_POINT ( 'NONE',  ( -13.87470602645761986, 4.985154336109792972, 4.916666666666650087 ) ) ;
#9960 = DIRECTION ( 'NONE',  ( 1.000000000000000000, 0.000000000000000000, 0.000000000000000000 ) ) ;
#9961 = CARTESIAN_POINT ( 'NONE',  ( 9.065941417683177406, -23.20159541128344927, 2.226721677130534705 ) ) ;
#9962 = CARTESIAN_POINT ( 'NONE',  ( -6.059058582316795949, -21.25705176302045274, 4.171265325393551215 ) ) ;
#9963 = ORIENTED_EDGE ( 'NONE', *, *, #154, .F. ) ;
#9964 = CARTESIAN_POINT ( 'NONE',  ( 13.90434039801927568, 5.731690099970989216, 5.115558489342345361 ) ) ;
#9965 = CARTESIAN_POINT ( 'NONE',  ( 13.12529397353891270, 5.014845663890295846, 3.333333333333220239 ) ) ;
#9966 = DIRECTION ( 'NONE',  ( 0.000000000000000000, 0.000000000000000000, 1.000000000000000000 ) ) ;
#9967 = ORIENTED_EDGE ( 'NONE', *, *, #1099, .T. ) ;
#9968 = ORIENTED_EDGE ( 'NONE', *, *, #7515, .T. ) ;
#9969 = DIRECTION ( 'NONE',  ( 1.000000000000000000, -2.312964634635752916E-15, 0.000000000000000000 ) ) ;
#9970 = LINE ( 'NONE', #16458, #9915 ) ;
#9971 = AXIS2_PLACEMENT_3D ( 'NONE', #3502, #16263, #17422 ) ;
#9972 = EDGE_CURVE ( 'NONE', #20148, #19218, #14554, .T. ) ;
#9973 = AXIS2_PLACEMENT_3D ( 'NONE', #3422, #14501, #4781 ) ;
#9974 = CARTESIAN_POINT ( 'NONE',  ( -14.49999999999998579, -25.49999999999999645, 4.000000000000000000 ) ) ;
#9975 = LINE ( 'NONE', #16356, #8993 ) ;
#9976 = CARTESIAN_POINT ( 'NONE',  ( 1.709849555000590104, -9.864920124259167977, 1.622644547201689713 ) ) ;
#9977 = CARTESIAN_POINT ( 'NONE',  ( -2.061130159782011972, 0.000000000000000000, 0.000000000000000000 ) ) ;
#9978 = CARTESIAN_POINT ( 'NONE',  ( 0.000000000000000000, 9.000000000000001776, 1.000000000000000000 ) ) ;
#9979 = CARTESIAN_POINT ( 'NONE',  ( 13.12211305460728106, -20.60792114491041005, 3.483674240224274410 ) ) ;
#9980 = LINE ( 'NONE', #13424, #5978 ) ;
#9981 = CARTESIAN_POINT ( 'NONE',  ( -9.340308582316794173, -22.67418626127525982, 5.270995438708342640 ) ) ;
#9982 = VECTOR ( 'NONE', #17026, 1000.000000000000000 ) ;
#9983 = CARTESIAN_POINT ( 'NONE',  ( -1.728780693989796724, -8.364929292255887106, 2.372646901726390478 ) ) ;
#9984 = VECTOR ( 'NONE', #19411, 1000.000000000000000 ) ;
#9985 = ORIENTED_EDGE ( 'NONE', *, *, #18074, .T. ) ;
#9986 = CARTESIAN_POINT ( 'NONE',  ( -12.64917329730235096, -18.27924848622803466, 4.778345106674467324 ) ) ;
#9987 = CARTESIAN_POINT ( 'NONE',  ( -8.777808582316792396, -20.27099543870833642, 2.724438792969431589 ) ) ;
#9988 = ADVANCED_FACE ( 'NONE', ( #11015 ), #3372, .T. ) ;
#9989 = CARTESIAN_POINT ( 'NONE',  ( -5.315941417683176518, -20.79840458871654363, 4.773278322869464851 ) ) ;
#9990 = CIRCLE ( 'NONE', #5332, 1.499999999999998668 ) ;
#9991 = VERTEX_POINT ( 'NONE', #3168 ) ;
#9992 = CARTESIAN_POINT ( 'NONE',  ( 13.38090111944825367, -19.20199346786276351, 4.743968713382380464 ) ) ;
#9993 = CARTESIAN_POINT ( 'NONE',  ( -0.000000000000000000, 11.64110105645932691, 0.000000000000000000 ) ) ;
#9994 = EDGE_LOOP ( 'NONE', ( #16422, #13254, #3277, #15345 ) ) ;
#9995 = ORIENTED_EDGE ( 'NONE', *, *, #6971, .T. ) ;
#9996 = CARTESIAN_POINT ( 'NONE',  ( -11.24178095869206828, 9.000000000000001776, 0.000000000000000000 ) ) ;
#9997 = ORIENTED_EDGE ( 'NONE', *, *, #4034, .T. ) ;
#9998 = CARTESIAN_POINT ( 'NONE',  ( 8.119520639128047890, 0.000000000000000000, 0.000000000000000000 ) ) ;
#9999 = ADVANCED_FACE ( 'NONE', ( #9751 ), #8187, .T. ) ;
#10000 = EDGE_CURVE ( 'NONE', #4871, #6936, #9441, .T. ) ;
#10001 = VECTOR ( 'NONE', #14576, 1000.000000000000000 ) ;
#10002 = ORIENTED_EDGE ( 'NONE', *, *, #8063, .F. ) ;
#10003 = CARTESIAN_POINT ( 'NONE',  ( 7.284691417683176518, -23.77099543870834353, 4.174186261275251830 ) ) ;
#10004 = DIRECTION ( 'NONE',  ( 0.000000000000000000, -0.000000000000000000, -1.000000000000000000 ) ) ;
#10005 = VECTOR ( 'NONE', #3085, 1000.000000000000000 ) ;
#10006 = CARTESIAN_POINT ( 'NONE',  ( -13.87490072368896676, 4.990068513505961256, 3.999999999999998224 ) ) ;
#10007 = LINE ( 'NONE', #5294, #17675 ) ;
#10008 = CARTESIAN_POINT ( 'NONE',  ( -4.746558582316793284, -21.94931252712234482, 5.250000000000000888 ) ) ;
#10009 = CARTESIAN_POINT ( 'NONE',  ( 0.000000000000000000, 9.000000000000001776, 1.000000000000000000 ) ) ;
#10010 = CARTESIAN_POINT ( 'NONE',  ( 9.440941417683177406, -20.72672167713052715, 2.298404588716546293 ) ) ;
#10011 = CARTESIAN_POINT ( 'NONE',  ( -17.55017143803810242, 0.000000000000000000, 0.000000000000000000 ) ) ;
#10012 = CARTESIAN_POINT ( 'NONE',  ( -10.00344141768317741, -22.05068747287766229, 4.499999999999999112 ) ) ;
#10013 = EDGE_CURVE ( 'NONE', #17944, #4108, #7872, .T. ) ;
#10014 = CARTESIAN_POINT ( 'NONE',  ( -10.84030858231679595, -22.98484643305508612, 6.020995438708344416 ) ) ;
#10015 = ORIENTED_EDGE ( 'NONE', *, *, #1394, .F. ) ;
#10016 = CARTESIAN_POINT ( 'NONE',  ( 12.62499999999998224, -20.24999999999991829, 4.333333333333343695 ) ) ;
#10017 = CARTESIAN_POINT ( 'NONE',  ( -12.62745083560477966, -20.12623280195927933, 5.001038150054709419 ) ) ;
#10018 = VECTOR ( 'NONE', #15814, 1000.000000000000000 ) ;
#10019 = VERTEX_POINT ( 'NONE', #1703 ) ;
#10020 = DIRECTION ( 'NONE',  ( -1.734723475976807094E-15, -1.000000000000000000, 0.000000000000000000 ) ) ;
#10021 = CARTESIAN_POINT ( 'NONE',  ( -22.06633994409548194, 0.000000000000000000, 0.000000000000000000 ) ) ;
#10022 = MECHANICAL_DESIGN_GEOMETRIC_PRESENTATION_REPRESENTATION (  '', ( #10367 ), #3042 ) ;
#10023 = VERTEX_POINT ( 'NONE', #9640 ) ;
#10024 = APPLICATION_PROTOCOL_DEFINITION ( 'draft international standard', 'automotive_design', 1998, #20183 ) ;
#10025 = ORIENTED_EDGE ( 'NONE', *, *, #1907, .T. ) ;
#10026 = VECTOR ( 'NONE', #9090, 1000.000000000000000 ) ;
#10027 = CARTESIAN_POINT ( 'NONE',  ( 13.37327929115833669, -20.24999999707183207, 3.449077790995325632 ) ) ;
#10028 = ORIENTED_EDGE ( 'NONE', *, *, #9922, .F. ) ;
#10029 = EDGE_CURVE ( 'NONE', #7911, #10437, #5323, .T. ) ;
#10030 = CYLINDRICAL_SURFACE ( 'NONE', #6944, 1.499999999999996891 ) ;
#10031 = CARTESIAN_POINT ( 'NONE',  ( 13.11514659413808737, 4.502403003978772134, 5.887634658581065494 ) ) ;
#10032 = CARTESIAN_POINT ( 'NONE',  ( -15.87779268661489773, 0.000000000000000000, 0.000000000000000000 ) ) ;
#10033 = VECTOR ( 'NONE', #13783, 1000.000000000000000 ) ;
#10034 = CARTESIAN_POINT ( 'NONE',  ( 12.62503117662529739, -20.24842558042254836, 4.565011198945062354 ) ) ;
#10035 = PRODUCT_DEFINITION_FORMATION_WITH_SPECIFIED_SOURCE ( 'ANY', '', #1835, .NOT_KNOWN. ) ;
#10036 = CARTESIAN_POINT ( 'NONE',  ( -27.52582389412042474, 4.853545418763153485, 1.000000000000000000 ) ) ;
#10037 = CARTESIAN_POINT ( 'NONE',  ( 12.90280858231679595, -23.08622137881038938, 1.020995438708339309 ) ) ;
#10038 = CARTESIAN_POINT ( 'NONE',  ( -13.10745701327265778, 3.364079170269163921, 6.743850412489304169 ) ) ;
#10039 = VECTOR ( 'NONE', #6136, 1000.000000000000000 ) ;
#10040 = CARTESIAN_POINT ( 'NONE',  ( -10.94094141768317741, -20.19639159124061933, 1.768074502826635586 ) ) ;
#10041 = VECTOR ( 'NONE', #12193, 1000.000000000000000 ) ;
#10042 = ADVANCED_FACE ( 'NONE', ( #6413 ), #14935, .T. ) ;
#10043 = ADVANCED_FACE ( 'NONE', ( #11117 ), #15913, .T. ) ;
#10044 = DIRECTION ( 'NONE',  ( -1.000000000000000000, -6.938893903907232322E-16, 0.000000000000000000 ) ) ;
#10045 = CARTESIAN_POINT ( 'NONE',  ( 0.3749999999999968914, 4.999999999999999112, 0.000000000000000000 ) ) ;
#10046 = CARTESIAN_POINT ( 'NONE',  ( 11.77780858231679595, -21.02099543870833998, 3.035098964749253003 ) ) ;
#10047 = CARTESIAN_POINT ( 'NONE',  ( -4.284691417683176518, -23.77099543870834353, 4.174186261275251830 ) ) ;
#10048 = VERTEX_POINT ( 'NONE', #14342 ) ;
#10049 = ADVANCED_FACE ( 'NONE', ( #26 ), #19181, .T. ) ;
#10050 = ORIENTED_EDGE ( 'NONE', *, *, #20641, .T. ) ;
#10051 = CARTESIAN_POINT ( 'NONE',  ( 13.87215786865436762, 4.856472367046606564, 5.506273593909547515 ) ) ;
#10052 = CARTESIAN_POINT ( 'NONE',  ( 13.50000000000001243, -19.49999999999999645, 4.000000000000000000 ) ) ;
#10053 = ORIENTED_EDGE ( 'NONE', *, *, #9739, .F. ) ;
#10054 = PLANE ( 'NONE',  #16798 ) ;
#10055 = AXIS2_PLACEMENT_3D ( 'NONE', #5129, #5225, #10044 ) ;
#10056 = CARTESIAN_POINT ( 'NONE',  ( -20.00000000000000000, -6.000000000000000000, 2.000000000000000000 ) ) ;
#10057 = AXIS2_PLACEMENT_3D ( 'NONE', #10830, #20562, #18669 ) ;
#10058 = EDGE_CURVE ( 'NONE', #14903, #13849, #14450, .T. ) ;
#10059 = DIRECTION ( 'NONE',  ( 1.000000000000000000, 0.000000000000000000, 0.000000000000000000 ) ) ;
#10060 = VECTOR ( 'NONE', #9960, 1000.000000000000000 ) ;
#10061 = CARTESIAN_POINT ( 'NONE',  ( 13.54769662923970763, -11.52882022337116119, 5.659013032956382361 ) ) ;
#10062 = VECTOR ( 'NONE', #12143, 1000.000000000000000 ) ;
#10063 = FACE_BOUND ( 'NONE', #6141, .T. ) ;
#10064 = CARTESIAN_POINT ( 'NONE',  ( 3.173374397671306912, -9.279487642487616483, 2.607523756204581211 ) ) ;
#10065 = CARTESIAN_POINT ( 'NONE',  ( 0.2815691515810352930, -9.114917468222230923, 1.622643865078524206 ) ) ;
#10066 = CARTESIAN_POINT ( 'NONE',  ( -12.62525331949183105, -19.48720736566255951, 4.581880915780448760 ) ) ;
#10067 = CARTESIAN_POINT ( 'NONE',  ( 8.777808582316792396, -20.27099543870833642, 2.724438792969431589 ) ) ;
#10068 = CARTESIAN_POINT ( 'NONE',  ( -15.61404127825609223, 4.999999999999999112, 0.000000000000000000 ) ) ;
#10069 = CARTESIAN_POINT ( 'NONE',  ( 13.10192273101908000, 3.834597916462216816, 6.003936301248457674 ) ) ;
#10070 = CARTESIAN_POINT ( 'NONE',  ( -2.702705060698113115, -10.69015907548275379, 2.777197378435510622 ) ) ;
#10071 = CARTESIAN_POINT ( 'NONE',  ( 7.184058582316795949, -21.32873467460644079, 2.757051763020455404 ) ) ;
#10072 = AXIS2_PLACEMENT_3D ( 'NONE', #4300, #10581, #5875 ) ;
#10073 = CARTESIAN_POINT ( 'NONE',  ( 11.40969141768318096, -21.32581373872474373, 5.270995438708348857 ) ) ;
#10074 = CARTESIAN_POINT ( 'NONE',  ( -10.27780858231679595, -21.02099543870833998, 3.035098964749253003 ) ) ;
#10075 = EDGE_LOOP ( 'NONE', ( #15978, #9324, #19241, #14599 ) ) ;
#10076 = CARTESIAN_POINT ( 'NONE',  ( 12.62500000000002132, -21.00000000000274269, 4.083333333315724012 ) ) ;
#10077 = CARTESIAN_POINT ( 'NONE',  ( 12.62499999999998401, -19.49999999999998934, 2.439580858552613751 ) ) ;
#10078 = CARTESIAN_POINT ( 'NONE',  ( -13.09878990694840795, -19.87505979123735500, 3.486523226841349743 ) ) ;
#10079 = ORIENTED_EDGE ( 'NONE', *, *, #8544, .T. ) ;
#10080 = ORIENTED_EDGE ( 'NONE', *, *, #9648, .T. ) ;
#10081 = LINE ( 'NONE', #5370, #1432 ) ;
#10082 = EDGE_CURVE ( 'NONE', #13278, #18598, #5431, .T. ) ;
#10083 = CARTESIAN_POINT ( 'NONE',  ( 2.693754455098655409, -9.955255285363838524, 2.600628789231445470 ) ) ;
#10084 = LINE ( 'NONE', #6640, #14303 ) ;
#10085 = VECTOR ( 'NONE', #7856, 1000.000000000000000 ) ;
#10086 = CARTESIAN_POINT ( 'NONE',  ( -18.98630159782011262, 4.999999999999999112, 1.000000000000000000 ) ) ;
#10087 = CARTESIAN_POINT ( 'NONE',  ( 1.126276606324276619, -9.114917468222230923, 2.372643865078341019 ) ) ;
#10088 = CARTESIAN_POINT ( 'NONE',  ( 20.00000000000000000, 3.000000000000004441, 2.000000000000000000 ) ) ;
#10089 = DIRECTION ( 'NONE',  ( 0.000000000000000000, -1.000000000000000000, 0.000000000000000000 ) ) ;
#10090 = DIRECTION ( 'NONE',  ( 0.000000000000000000, -0.000000000000000000, -1.000000000000000000 ) ) ;
#10091 = CARTESIAN_POINT ( 'NONE',  ( -1.957016269584227031, -9.152392576945766578, 2.382268221639079364 ) ) ;
#10092 = CARTESIAN_POINT ( 'NONE',  ( -7.746558582316794173, -21.94931252712234482, 5.250000000000000888 ) ) ;
#10093 = CARTESIAN_POINT ( 'NONE',  ( -3.767139617958116471, -12.99583330722436791, 3.561955564372631500 ) ) ;
#10094 = EDGE_LOOP ( 'NONE', ( #15339, #7513, #9156, #17709 ) ) ;
#10095 = CARTESIAN_POINT ( 'NONE',  ( -13.37499999999998224, -19.49999999999991473, 4.333333333333343695 ) ) ;
#10096 = CARTESIAN_POINT ( 'NONE',  ( -5.965308582316793284, -20.22900456129164937, 4.174186261275266929 ) ) ;
#10097 = CARTESIAN_POINT ( 'NONE',  ( -6.440941417683176518, -20.72672167713052715, 2.298404588716546293 ) ) ;
#10098 = ORIENTED_EDGE ( 'NONE', *, *, #5955, .F. ) ;
#10099 = CARTESIAN_POINT ( 'NONE',  ( 13.84501469867711698, 4.235742283194553259, 3.666666666666500873 ) ) ;
#10100 = VERTEX_POINT ( 'NONE', #10235 ) ;
#10101 = VERTEX_POINT ( 'NONE', #15041 ) ;
#10102 = VECTOR ( 'NONE', #5189, 1000.000000000000000 ) ;
#10103 = DIRECTION ( 'NONE',  ( 1.000000000000000000, 0.000000000000000000, 0.000000000000000000 ) ) ;
#10104 = ORIENTED_EDGE ( 'NONE', *, *, #5944, .T. ) ;
#10105 = CARTESIAN_POINT ( 'NONE',  ( 0.000000000000000000, 16.00000000000000000, 1.000000000000000000 ) ) ;
#10106 = B_SPLINE_CURVE_WITH_KNOTS ( 'NONE', 3,
 ( #19929, #13527, #11756, #11957, #19615, #18147, #18248, #2039, #8521, #473, #13216, #16773, #3711, #10091, #16466, #19830, #3911, #10291, #16661, #4121, #18556, #13733, #1093, #5797, #2542, #6000, #12168, #8930, #5693, #20237 ),
 .UNSPECIFIED., .F., .F.,
 ( 4, 2, 2, 2, 2, 2, 2, 2, 2, 2, 2, 2, 2, 2, 4 ),
 ( 0.6078525888943429045, 0.6200887121040892236, 0.6309950902025724950, 0.6419014683010558775, 0.6637142244980225314, 0.7073397368919559502, 0.7509652492858893691, 0.7727780054828560230, 0.7836843835813394055, 0.7945907616798226769, 0.8074288390748337596, 0.8202669164698448423, 0.8459430712598670077, 0.8972953808399113385, 1.000000000000000000 ),
 .UNSPECIFIED. ) ;
#10107 = ORIENTED_EDGE ( 'NONE', *, *, #528, .T. ) ;
#10108 = CARTESIAN_POINT ( 'NONE',  ( 4.284691417683176518, -23.77099543870834353, 4.174186261275251830 ) ) ;
#10109 = CARTESIAN_POINT ( 'NONE',  ( -13.49999999999998401, -21.99999999999999645, 11.68378559369222280 ) ) ;
#10110 = EDGE_CURVE ( 'NONE', #8456, #6003, #15150, .T. ) ;
#10111 = CARTESIAN_POINT ( 'NONE',  ( 9.000000000000000000, -9.999999999999991118, 2.500000000000000000 ) ) ;
#10112 = CARTESIAN_POINT ( 'NONE',  ( 3.162271481458107658, -13.95306990448253437, 3.615178062515473911 ) ) ;
#10113 = CARTESIAN_POINT ( 'NONE',  ( 0.000000000000000000, 4.999999999999999112, 0.000000000000000000 ) ) ;
#10114 = VECTOR ( 'NONE', #19708, 1000.000000000000000 ) ;
#10115 = CARTESIAN_POINT ( 'NONE',  ( 13.90439735423812273, 5.734566389025032684, 4.833333333333343695 ) ) ;
#10116 = CARTESIAN_POINT ( 'NONE',  ( 15.00000000000001421, -29.99999999999998579, 1.000000000000000000 ) ) ;
#10117 = EDGE_CURVE ( 'NONE', #19407, #2924, #13672, .T. ) ;
#10118 = EDGE_CURVE ( 'NONE', #16102, #2930, #11802, .T. ) ;
#10119 = CARTESIAN_POINT ( 'NONE',  ( 10.84719141768317563, -21.22443879296941915, 1.770995438708345748 ) ) ;
#10120 = CARTESIAN_POINT ( 'NONE',  ( 5.381197846483058989, -6.000000000000000000, 2.000000000000000000 ) ) ;
#10121 = CARTESIAN_POINT ( 'NONE',  ( -6.628441417683177406, -20.99999999999999645, 3.550687472877664952 ) ) ;
#10122 = CARTESIAN_POINT ( 'NONE',  ( -9.246558582316795949, -21.94931252712234127, 6.000000000000001776 ) ) ;
#10123 = ORIENTED_EDGE ( 'NONE', *, *, #20656, .T. ) ;
#10124 = CARTESIAN_POINT ( 'NONE',  ( 12.62499999999998224, -20.25000000000006395, 4.416666666666681174 ) ) ;
#10125 = CARTESIAN_POINT ( 'NONE',  ( -13.15452713448031297, 5.741120291255121799, 5.290164123766007087 ) ) ;
#10126 = ORIENTED_EDGE ( 'NONE', *, *, #8886, .F. ) ;
#10127 = CARTESIAN_POINT ( 'NONE',  ( 0.000000000000000000, 10.00000000000000000, 1.000000000000000000 ) ) ;
#10128 = CARTESIAN_POINT ( 'NONE',  ( -15.11404127825609223, 4.999999999999999112, 1.000000000000000000 ) ) ;
#10129 = ORIENTED_EDGE ( 'NONE', *, *, #10578, .F. ) ;
#10130 = ORIENTED_EDGE ( 'NONE', *, *, #18205, .T. ) ;
#10131 = VECTOR ( 'NONE', #19558, 1000.000000000000000 ) ;
#10132 = FACE_BOUND ( 'NONE', #7487, .T. ) ;
#10133 = ORIENTED_EDGE ( 'NONE', *, *, #11895, .T. ) ;
#10134 = CARTESIAN_POINT ( 'NONE',  ( 14.50000000000000000, -23.00000000000001421, 4.000000000000000000 ) ) ;
#10135 = CARTESIAN_POINT ( 'NONE',  ( 13.10012427866737639, 3.743776072700027324, 6.001983176248468332 ) ) ;
#10136 = ADVANCED_FACE ( 'NONE', ( #12217 ), #10550, .F. ) ;
#10137 = CARTESIAN_POINT ( 'NONE',  ( -1.798207051321043304, -8.367281747657623114, 1.623251059268568053 ) ) ;
#10138 = DIRECTION ( 'NONE',  ( 1.000000000000000000, 0.000000000000000000, -0.000000000000000000 ) ) ;
#10139 = LINE ( 'NONE', #7110, #11794 ) ;
#10140 = CARTESIAN_POINT ( 'NONE',  ( 12.63819864697926754, -19.58346832754827105, 5.450273968536036406 ) ) ;
#10141 = CARTESIAN_POINT ( 'NONE',  ( 17.12779268661489596, 10.00000000000000000, 1.000000000000000000 ) ) ;
#10142 = EDGE_CURVE ( 'NONE', #3140, #6097, #7209, .T. ) ;
#10143 = ADVANCED_FACE ( 'NONE', ( #12008 ), #7109, .T. ) ;
#10144 = CARTESIAN_POINT ( 'NONE',  ( 12.80905858231679417, -23.80360840875935935, 1.768074502826626260 ) ) ;
#10145 = CARTESIAN_POINT ( 'NONE',  ( -12.62524871736568954, -20.23743977303344010, 4.661898514667671023 ) ) ;
#10146 = CARTESIAN_POINT ( 'NONE',  ( -9.253441417683177406, -21.94931252712233061, 0.9999999999999978906 ) ) ;
#10147 = CARTESIAN_POINT ( 'NONE',  ( -2.499999999999998668, -19.50000000000000000, 1.000000000000000000 ) ) ;
#10148 = CARTESIAN_POINT ( 'NONE',  ( 25.37918902992234393, 0.000000000000000000, 1.000000000000000000 ) ) ;
#10149 = CARTESIAN_POINT ( 'NONE',  ( 9.809058582316795949, -22.74294823697954016, 2.828734674606448785 ) ) ;
#10150 = CARTESIAN_POINT ( 'NONE',  ( -13.87500000000000000, 5.000000000000049738, 4.000000000000000888 ) ) ;
#10151 = ORIENTED_EDGE ( 'NONE', *, *, #5330, .F. ) ;
#10152 = ORIENTED_EDGE ( 'NONE', *, *, #18519, .F. ) ;
#10153 = CARTESIAN_POINT ( 'NONE',  ( 13.85223456079946303, 3.850345320370711644, 5.989742199623227847 ) ) ;
#10154 = DIRECTION ( 'NONE',  ( 0.000000000000000000, 1.000000000000000000, 0.000000000000000000 ) ) ;
#10155 = ORIENTED_EDGE ( 'NONE', *, *, #3876, .T. ) ;
#10156 = LINE ( 'NONE', #17802, #3442 ) ;
#10157 = VECTOR ( 'NONE', #3548, 1000.000000000000000 ) ;
#10158 = DIRECTION ( 'NONE',  ( 0.000000000000000000, -0.000000000000000000, 1.000000000000000000 ) ) ;
#10159 = LINE ( 'NONE', #19897, #12985 ) ;
#10160 = CARTESIAN_POINT ( 'NONE',  ( 13.85723511636018301, 4.102873376188801657, 5.986996695041598926 ) ) ;
#10161 = EDGE_CURVE ( 'NONE', #12873, #8157, #4067, .T. ) ;
#10162 = EDGE_CURVE ( 'NONE', #17800, #3061, #5530, .T. ) ;
#10163 = LINE ( 'NONE', #6915, #17539 ) ;
#10164 = CARTESIAN_POINT ( 'NONE',  ( 3.292205091070697698, -9.639507599131205140, 2.699984073191874057 ) ) ;
#10165 = CARTESIAN_POINT ( 'NONE',  ( -17.94064177244175795, 10.00000000000000000, 0.000000000000000000 ) ) ;
#10166 = CARTESIAN_POINT ( 'NONE',  ( -13.05202662408965075, 2.064844516520778939, 5.215845106673912213 ) ) ;
#10167 = CARTESIAN_POINT ( 'NONE',  ( -5.999999999999999112, -2.500000000000047518, 9.999999999999998224 ) ) ;
#10168 = CARTESIAN_POINT ( 'NONE',  ( 0.000000000000000000, 9.000000000000001776, 0.000000000000000000 ) ) ;
#10169 = CARTESIAN_POINT ( 'NONE',  ( 12.72125031657057015, -15.38935901321805133, 5.590524842915047365 ) ) ;
#10170 = DIRECTION ( 'NONE',  ( -1.000000000000000000, 0.000000000000000000, 0.000000000000000000 ) ) ;
#10171 = CARTESIAN_POINT ( 'NONE',  ( 9.621558582316795949, -22.99999999999999645, 3.550687472877652073 ) ) ;
#10172 = CARTESIAN_POINT ( 'NONE',  ( 7.284691417683176518, -23.77099543870834353, 4.174186261275252718 ) ) ;
#10173 = CARTESIAN_POINT ( 'NONE',  ( -8.215308582316792396, -23.77099543870833998, 2.825813738724734847 ) ) ;
#10174 = ORIENTED_EDGE ( 'NONE', *, *, #6345, .T. ) ;
#10175 = CARTESIAN_POINT ( 'NONE',  ( 13.12035191997235906, 4.015271958632619764, 6.757839745787993735 ) ) ;
#10176 = CARTESIAN_POINT ( 'NONE',  ( 13.04243487821393721, 1.580461349787872782, 5.205428440007538349 ) ) ;
#10177 = DIRECTION ( 'NONE',  ( 0.000000000000000000, -1.000000000000000000, 0.000000000000000000 ) ) ;
#10178 = ORIENTED_EDGE ( 'NONE', *, *, #4000, .F. ) ;
#10179 = ORIENTED_EDGE ( 'NONE', *, *, #7884, .T. ) ;
#10180 = DIRECTION ( 'NONE',  ( -1.000000000000000000, 6.938893903907222067E-15, 0.000000000000000000 ) ) ;
#10181 = DIRECTION ( 'NONE',  ( 0.000000000000000000, -0.000000000000000000, -1.000000000000000000 ) ) ;
#10182 = ADVANCED_FACE ( 'NONE', ( #16823 ), #19875, .T. ) ;
#10183 = EDGE_CURVE ( 'NONE', #3797, #17356, #10652, .T. ) ;
#10184 = CARTESIAN_POINT ( 'NONE',  ( 14.50000000000001243, -18.49999999999999645, 4.000000000000000000 ) ) ;
#10185 = FACE_OUTER_BOUND ( 'NONE', #10522, .T. ) ;
#10186 = CARTESIAN_POINT ( 'NONE',  ( 3.047379876266447685, -13.13734219723468755, 3.405682891496055742 ) ) ;
#10187 = CARTESIAN_POINT ( 'NONE',  ( -13.49999999999998401, -18.49999999999999645, 4.000000000000000000 ) ) ;
#10188 = LINE ( 'NONE', #8730, #5056 ) ;
#10189 = CARTESIAN_POINT ( 'NONE',  ( 13.37327929115833669, -20.24999999707183207, 3.449077790995325632 ) ) ;
#10190 = CARTESIAN_POINT ( 'NONE',  ( -17.11324865405191176, -11.00000000000000000, 2.000000000000000000 ) ) ;
#10191 = CARTESIAN_POINT ( 'NONE',  ( -7.465308582316795061, -20.22900456129164937, 4.174186261275266929 ) ) ;
#10192 = CARTESIAN_POINT ( 'NONE',  ( -3.528325504133930313, -10.14411005961392398, 2.079576065490765124 ) ) ;
#10193 = VERTEX_POINT ( 'NONE', #18605 ) ;
#10194 = CARTESIAN_POINT ( 'NONE',  ( -13.37514942709654164, -19.49245393162283690, 4.562067678168288509 ) ) ;
#10195 = CARTESIAN_POINT ( 'NONE',  ( -6.340308582316793284, -22.67418626127525982, 5.270995438708342640 ) ) ;
#10196 = EDGE_CURVE ( 'NONE', #1434, #6863, #15353, .T. ) ;
#10197 = CARTESIAN_POINT ( 'NONE',  ( -4.847191417683178294, -21.22443879296941915, 1.770995438708345748 ) ) ;
#10198 = ORIENTED_EDGE ( 'NONE', *, *, #18228, .T. ) ;
#10199 = CARTESIAN_POINT ( 'NONE',  ( 13.37524505148396514, -20.23762490005974968, 4.659512268729234741 ) ) ;
#10201 = CARTESIAN_POINT ( 'NONE',  ( -24.50000000000000000, 0.000000000000000000, 1.000000000000000000 ) ) ;
#10200 = VECTOR ( 'NONE', #18218, 1000.000000000000000 ) ;
#10202 = ORIENTED_EDGE ( 'NONE', *, *, #19635, .F. ) ;
#10203 = AXIS2_PLACEMENT_3D ( 'NONE', #15713, #4324, #5892 ) ;
#10204 = ORIENTED_EDGE ( 'NONE', *, *, #9662, .F. ) ;
#10205 = PLANE ( 'NONE',  #9715 ) ;
#10206 = ORIENTED_EDGE ( 'NONE', *, *, #18743, .T. ) ;
#10207 = LINE ( 'NONE', #9998, #3415 ) ;
#10208 = ORIENTED_EDGE ( 'NONE', *, *, #16334, .T. ) ;
#10209 = CARTESIAN_POINT ( 'NONE',  ( 6.815941417683176518, -20.79840458871654363, 4.773278322869464851 ) ) ;
#10210 = CARTESIAN_POINT ( 'NONE',  ( -15.49999999999999822, -20.99999999999999645, 4.000000000000000000 ) ) ;
#10211 = DIRECTION ( 'NONE',  ( -0.000000000000000000, -0.000000000000000000, -1.000000000000000000 ) ) ;
#10212 = CARTESIAN_POINT ( 'NONE',  ( 3.564229130755586006, -10.39902496812945465, 2.145043306434553987 ) ) ;
#10213 = CARTESIAN_POINT ( 'NONE',  ( -6.996558582316793284, -22.05068747287764452, 1.749999999999998446 ) ) ;
#10214 = CARTESIAN_POINT ( 'NONE',  ( 12.62499999999998224, -20.99999999999998934, 4.291666666666699825 ) ) ;
#10215 = DIRECTION ( 'NONE',  ( -1.000000000000000000, 0.000000000000000000, 0.000000000000000000 ) ) ;
#10216 = CARTESIAN_POINT ( 'NONE',  ( 10.28469141768317741, -23.02099543870834353, 3.863526089495429972 ) ) ;
#10217 = CARTESIAN_POINT ( 'NONE',  ( -12.62500000000001954, -20.24999999999450040, 3.833333333368183382 ) ) ;
#10218 = CARTESIAN_POINT ( 'NONE',  ( -6.347191417683176518, -21.53509896474923835, 2.520995438708346192 ) ) ;
#10219 = CARTESIAN_POINT ( 'NONE',  ( -10.18405858231679595, -20.26807450282662160, 1.696391591240633101 ) ) ;
#10220 = ORIENTED_EDGE ( 'NONE', *, *, #12428, .F. ) ;
#10221 = CARTESIAN_POINT ( 'NONE',  ( 12.62746768552656285, -19.37538188090202596, 4.723115281690125400 ) ) ;
#10222 = CARTESIAN_POINT ( 'NONE',  ( -13.12175473207386922, 4.086113969730903683, 6.756475741440692850 ) ) ;
#10223 = ORIENTED_EDGE ( 'NONE', *, *, #14932, .T. ) ;
#10224 = EDGE_CURVE ( 'NONE', #3395, #15652, #7310, .T. ) ;
#10225 = LINE ( 'NONE', #8353, #18979 ) ;
#10226 = CARTESIAN_POINT ( 'NONE',  ( -5.381197846483055436, -6.000000000000000000, 1.000000000000000000 ) ) ;
#10227 = VERTEX_POINT ( 'NONE', #2592 ) ;
#10228 = ITEM_DEFINED_TRANSFORMATION ( 'NONE', 'NONE', #8709,  #18039 ) ;
#10229 = VERTEX_POINT ( 'NONE', #7520 ) ;
#10230 = CARTESIAN_POINT ( 'NONE',  ( 12.93505857549037863, -19.87496680839758056, 3.508858656608841997 ) ) ;
#10231 = VERTEX_POINT ( 'NONE', #13884 ) ;
#10232 = CARTESIAN_POINT ( 'NONE',  ( 5.999999999999999112, -7.500000000000047073, 2.000000000000000000 ) ) ;
#10233 = CARTESIAN_POINT ( 'NONE',  ( 13.12529397354238192, 5.014845663890295846, 4.916666666666650087 ) ) ;
#10234 = CARTESIAN_POINT ( 'NONE',  ( -2.887553741010006281, -10.84643174835951207, 2.067331322690557638 ) ) ;
#10235 = CARTESIAN_POINT ( 'NONE',  ( -17.55017143803810242, 4.999999999999999112, 1.000000000000000000 ) ) ;
#10236 = LINE ( 'NONE', #3760, #16149 ) ;
#10237 = CARTESIAN_POINT ( 'NONE',  ( -24.50000000000000000, 3.000000000000000888, 1.000000000000000000 ) ) ;
#10238 = CARTESIAN_POINT ( 'NONE',  ( -14.56494360078803396, 10.00000000000000000, 0.000000000000000000 ) ) ;
#10239 = CARTESIAN_POINT ( 'NONE',  ( 6.246558582316795949, -21.94931252712234127, 6.000000000000001776 ) ) ;
#10240 = CARTESIAN_POINT ( 'NONE',  ( -13.02818618459764188, 0.1109023222084986743, 5.923858176248589125 ) ) ;
#10241 = CARTESIAN_POINT ( 'NONE',  ( -7.753441417683177406, -21.94931252712233061, 0.9999999999999978906 ) ) ;
#10242 = ORIENTED_EDGE ( 'NONE', *, *, #20429, .F. ) ;
#10243 = PLANE ( 'NONE',  #9292 ) ;
#10244 = DIRECTION ( 'NONE',  ( 0.000000000000000000, 0.000000000000000000, 1.000000000000000000 ) ) ;
#10245 = EDGE_CURVE ( 'NONE', #4291, #378, #8671, .T. ) ;
#10246 = CARTESIAN_POINT ( 'NONE',  ( 11.49655858231679595, -22.05068747287764452, 2.499999999999999112 ) ) ;
#10247 = CARTESIAN_POINT ( 'NONE',  ( -14.49999999999998579, -24.49999999999999289, 1.000000000000000000 ) ) ;
#10248 = ORIENTED_EDGE ( 'NONE', *, *, #10789, .F. ) ;
#10249 = VERTEX_POINT ( 'NONE', #8979 ) ;
#10250 = CARTESIAN_POINT ( 'NONE',  ( 13.85723511636018301, 4.102873376188801657, 5.986996695041598926 ) ) ;
#10251 = LINE ( 'NONE', #5138, #2091 ) ;
#10252 =( NAMED_UNIT ( * ) PLANE_ANGLE_UNIT ( ) SI_UNIT ( $, .RADIAN. ) );
#10253 = ORIENTED_EDGE ( 'NONE', *, *, #4405, .T. ) ;
#10254 = DIRECTION ( 'NONE',  ( 0.000000000000000000, 1.000000000000000000, -0.000000000000000000 ) ) ;
#10255 = ADVANCED_FACE ( 'NONE', ( #3955 ), #1035, .T. ) ;
#10257 = EDGE_CURVE ( 'NONE', #7202, #5157, #16713, .T. ) ;
#10256 = VECTOR ( 'NONE', #16651, 1000.000000000000000 ) ;
#10258 = DIRECTION ( 'NONE',  ( 0.000000000000000000, 1.000000000000000000, 0.000000000000000000 ) ) ;
#10259 = CARTESIAN_POINT ( 'NONE',  ( 0.000000000000000000, 9.000000000000001776, 0.000000000000000000 ) ) ;
#10260 = CARTESIAN_POINT ( 'NONE',  ( 13.37499999999998224, -20.24999999999998934, 4.291666666666698937 ) ) ;
#10261 = CARTESIAN_POINT ( 'NONE',  ( -14.99999999999999645, -30.00000000000000711, 1.000000000000000000 ) ) ;
#10262 = CARTESIAN_POINT ( 'NONE',  ( 3.779650890485476200, -11.92851441922421607, 2.537846752097290715 ) ) ;
#10263 = CARTESIAN_POINT ( 'NONE',  ( 1.754777266914451461, -9.116337928146160507, 1.623008667563337726 ) ) ;
#10264 = CARTESIAN_POINT ( 'NONE',  ( -13.12529397354238192, 5.014845663890295846, 4.916666666666650087 ) ) ;
#10265 = CARTESIAN_POINT ( 'NONE',  ( 6.996558582316793284, -22.05068747287764452, 1.749999999999998446 ) ) ;
#10266 = DIRECTION ( 'NONE',  ( 0.000000000000000000, 1.000000000000000000, 0.000000000000000000 ) ) ;
#10267 = CARTESIAN_POINT ( 'NONE',  ( 12.83635126708105823, -9.576761012430582198, 5.715524842913705328 ) ) ;
#10268 = CARTESIAN_POINT ( 'NONE',  ( 19.73630159782011617, 9.000000000000001776, 0.000000000000000000 ) ) ;
#10269 = CARTESIAN_POINT ( 'NONE',  ( 8.402808582316797725, -22.46490103525074034, 2.520995438708341307 ) ) ;
#10270 = EDGE_CURVE ( 'NONE', #7916, #10336, #5848, .T. ) ;
#10271 = CARTESIAN_POINT ( 'NONE',  ( 6.722191417683177406, -20.27099543870833998, 4.275561207030583510 ) ) ;
#10272 = CARTESIAN_POINT ( 'NONE',  ( -10.37155858231679417, -20.24999999999999289, 3.449312527122348371 ) ) ;
#10273 = ORIENTED_EDGE ( 'NONE', *, *, #8645, .T. ) ;
#10274 = CARTESIAN_POINT ( 'NONE',  ( 13.15452713448031297, 5.741120291255121799, 5.290164123766007087 ) ) ;
#10275 = CARTESIAN_POINT ( 'NONE',  ( 12.62500004114794372, -19.49999792202770621, 4.520295319612473328 ) ) ;
#10276 = CIRCLE ( 'NONE', #3585, 9.999999999999998224 ) ;
#10277 = FACE_OUTER_BOUND ( 'NONE', #2972, .T. ) ;
#10278 = EDGE_LOOP ( 'NONE', ( #17143, #17633, #20298, #19321, #18937 ) ) ;
#10279 = VERTEX_POINT ( 'NONE', #1242 ) ;
#10280 = PLANE ( 'NONE',  #10797 ) ;
#10281 = DIRECTION ( 'NONE',  ( 0.000000000000000000, 0.000000000000000000, 1.000000000000000000 ) ) ;
#10282 = AXIS2_PLACEMENT_3D ( 'NONE', #10451, #4375, #9086 ) ;
#10283 = DIRECTION ( 'NONE',  ( 1.000000000000000000, -0.000000000000000000, -0.000000000000000000 ) ) ;
#10284 = ADVANCED_FACE ( 'NONE', ( #7616 ), #13984, .T. ) ;
#10285 = LINE ( 'NONE', #18243, #14995 ) ;
#10286 = CARTESIAN_POINT ( 'NONE',  ( 2.875042468481914248, -11.91375063635796039, 3.091440134965714126 ) ) ;
#10287 = CARTESIAN_POINT ( 'NONE',  ( 5.999999999999999112, -2.500000000000047518, 2.000000000000000000 ) ) ;
#10288 = CARTESIAN_POINT ( 'NONE',  ( -13.67791111847408025, 4.999999999999999112, 1.000000000000000000 ) ) ;
#10289 = VECTOR ( 'NONE', #13773, 1000.000000000000000 ) ;
#10290 = CARTESIAN_POINT ( 'NONE',  ( 13.30134771663319704, -20.47916202560290699, 3.458891087130237185 ) ) ;
#10291 = CARTESIAN_POINT ( 'NONE',  ( -1.743623630681728542, -9.116095536440919744, 2.372946416531167557 ) ) ;
#10292 = CARTESIAN_POINT ( 'NONE',  ( -6.996558582316793284, -22.05068747287764452, 1.749999999999998446 ) ) ;
#10293 = CARTESIAN_POINT ( 'NONE',  ( -3.422464802389687311, -10.54865018547243061, 2.933470051312085936 ) ) ;
#10294 = EDGE_LOOP ( 'NONE', ( #10807, #12388, #18161, #19754 ) ) ;
#10295 = CARTESIAN_POINT ( 'NONE',  ( -13.09560264576187905, 4.265433610975056133, 4.583333333333295734 ) ) ;
#10296 = CARTESIAN_POINT ( 'NONE',  ( -8.965308582316794173, -20.22900456129164937, 4.174186261275266929 ) ) ;
#10297 = ADVANCED_FACE ( 'NONE', ( #6247 ), #4785, .T. ) ;
#10298 = CARTESIAN_POINT ( 'NONE',  ( 8.121558582316795949, -24.50000000000000000, 3.550687472877651629 ) ) ;
#10299 = CARTESIAN_POINT ( 'NONE',  ( -4.097191417683176518, -22.77556120703057729, 5.229004561291655584 ) ) ;
#10300 = ORIENTED_EDGE ( 'NONE', *, *, #3366, .T. ) ;
#10301 = ADVANCED_FACE ( 'NONE', ( #9185 ), #6156, .T. ) ;
#10302 = CARTESIAN_POINT ( 'NONE',  ( 13.37499979530394967, -20.25001033714808329, 4.458488164327452097 ) ) ;
#10303 = DIRECTION ( 'NONE',  ( 0.000000000000000000, 0.2487476929738665354, 0.9685683172808094987 ) ) ;
#10304 = ORIENTED_EDGE ( 'NONE', *, *, #2725, .T. ) ;
#10305 = VECTOR ( 'NONE', #3953, 1000.000000000000000 ) ;
#10306 = ORIENTED_EDGE ( 'NONE', *, *, #18217, .F. ) ;
#10307 = DIRECTION ( 'NONE',  ( -0.000000000000000000, -0.000000000000000000, -1.000000000000000000 ) ) ;
#10308 = AXIS2_PLACEMENT_3D ( 'NONE', #805, #7189, #5611 ) ;
#10309 = ORIENTED_EDGE ( 'NONE', *, *, #17569, .T. ) ;
#10310 = CARTESIAN_POINT ( 'NONE',  ( -13.39359219590679295, -19.31109410670777038, 5.491647114909025795 ) ) ;
#10311 = ORIENTED_EDGE ( 'NONE', *, *, #18090, .T. ) ;
#10312 = CARTESIAN_POINT ( 'NONE',  ( 5.315941417683176518, -20.79840458871654363, 4.773278322869464851 ) ) ;
#10313 = EDGE_CURVE ( 'NONE', #11223, #16474, #11170, .T. ) ;
#10314 = DIRECTION ( 'NONE',  ( 1.000000000000000000, 0.000000000000000000, 0.000000000000000000 ) ) ;
#10315 = DIRECTION ( 'NONE',  ( 1.000000000000000000, 0.000000000000000000, 0.000000000000000000 ) ) ;
#10316 = VECTOR ( 'NONE', #10315, 1000.000000000000000 ) ;
#10317 = CARTESIAN_POINT ( 'NONE',  ( 2.910499702382182807, -8.879427762644468203, 2.504780387061739333 ) ) ;
#10318 = CARTESIAN_POINT ( 'NONE',  ( -7.090308582316795061, -21.32581373872472952, 1.729004561291657138 ) ) ;
#10319 = VECTOR ( 'NONE', #4882, 1000.000000000000000 ) ;
#10320 = CARTESIAN_POINT ( 'NONE',  ( 13.90439735423812273, 5.734566389025032684, 4.333333333333380999 ) ) ;
#10321 = VECTOR ( 'NONE', #16898, 1000.000000000000000 ) ;
#10322 = LINE ( 'NONE', #16691, #12623 ) ;
#10323 = AXIS2_PLACEMENT_3D ( 'NONE', #15557, #1237, #1343 ) ;
#10324 = CARTESIAN_POINT ( 'NONE',  ( 4.847191417683178294, -21.22443879296941915, 1.770995438708345748 ) ) ;
#10325 = CARTESIAN_POINT ( 'NONE',  ( -12.64691428603184242, -19.14332855539073464, 5.509795676248469221 ) ) ;
#10326 = CARTESIAN_POINT ( 'NONE',  ( -5.784691417683178294, -23.02099543870834353, 3.863526089495429972 ) ) ;
#10327 = CARTESIAN_POINT ( 'NONE',  ( -10.65969141768317741, -22.98484643305507191, 0.9790045612916508100 ) ) ;
#10328 = ORIENTED_EDGE ( 'NONE', *, *, #11845, .F. ) ;
#10329 = CARTESIAN_POINT ( 'NONE',  ( 12.62958809053144549, -19.26830142816300295, 4.757073430686623361 ) ) ;
#10330 = CARTESIAN_POINT ( 'NONE',  ( -13.10192273101908000, 3.834597916462216816, 6.003936301248457674 ) ) ;
#10331 = EDGE_LOOP ( 'NONE', ( #3589, #4036, #6124, #15992 ) ) ;
#10332 = LINE ( 'NONE', #20071, #17966 ) ;
#10333 = CARTESIAN_POINT ( 'NONE',  ( -26.79469207716615387, 9.000000000000001776, 1.000000000000000000 ) ) ;
#10334 = ORIENTED_EDGE ( 'NONE', *, *, #19626, .T. ) ;
#10335 = VECTOR ( 'NONE', #13419, 1000.000000000000000 ) ;
#10336 = VERTEX_POINT ( 'NONE', #12621 ) ;
#10337 = VECTOR ( 'NONE', #14413, 1000.000000000000000 ) ;
#10338 = ORIENTED_EDGE ( 'NONE', *, *, #718, .F. ) ;
#10339 = LINE ( 'NONE', #13566, #7313 ) ;
#10340 = ADVANCED_FACE ( 'NONE', ( #20596 ), #20393, .F. ) ;
#10341 = CARTESIAN_POINT ( 'NONE',  ( 6.063547257480584207, 0.000000000000000000, 1.000000000000000000 ) ) ;
#10342 = CARTESIAN_POINT ( 'NONE',  ( -3.462011766956747394, -14.92507028461178287, 3.114807177791267812 ) ) ;
#10343 = DIRECTION ( 'NONE',  ( 0.000000000000000000, -1.000000000000000000, 0.000000000000000000 ) ) ;
#10344 = DIRECTION ( 'NONE',  ( 8.673617379884047798E-17, -1.000000000000000000, 0.000000000000000000 ) ) ;
#10345 = CARTESIAN_POINT ( 'NONE',  ( 19.23630159782011617, 0.000000000000000000, 1.000000000000000000 ) ) ;
#10346 = LINE ( 'NONE', #15460, #13023 ) ;
#10347 = CARTESIAN_POINT ( 'NONE',  ( 9.534691417683177406, -19.47900456129164581, 2.515153566944927199 ) ) ;
#10348 = CARTESIAN_POINT ( 'NONE',  ( -13.10012427866737639, 3.743776072700027324, 6.001983176248468332 ) ) ;
#10349 = CARTESIAN_POINT ( 'NONE',  ( -7.097191417683176518, -23.08622137881040359, 5.979004561291654696 ) ) ;
#10350 = VECTOR ( 'NONE', #2747, 1000.000000000000000 ) ;
#10351 = VERTEX_POINT ( 'NONE', #14189 ) ;
#10352 = CARTESIAN_POINT ( 'NONE',  ( 12.43405858231679417, -23.20159541128345992, 4.773278322869455970 ) ) ;
#10353 = LINE ( 'NONE', #4391, #5070 ) ;
#10354 = CARTESIAN_POINT ( 'NONE',  ( -13.86796007304617717, 3.894483688830428836, 6.740724019197413597 ) ) ;
#10355 = AXIS2_PLACEMENT_3D ( 'NONE', #19109, #8003, #2813 ) ;
#10356 = CARTESIAN_POINT ( 'NONE',  ( 4.746558582316795061, -21.94931252712234127, 4.499999999999999112 ) ) ;
#10357 = CARTESIAN_POINT ( 'NONE',  ( 5.381197846483058989, -14.00000000000000000, 1.000000000000000000 ) ) ;
#10358 = ORIENTED_EDGE ( 'NONE', *, *, #10000, .F. ) ;
#10359 = ORIENTED_EDGE ( 'NONE', *, *, #14456, .F. ) ;
#10360 = CARTESIAN_POINT ( 'NONE',  ( 13.87470602645761986, 4.985154336109792972, 4.666666666666619889 ) ) ;
#10361 = LINE ( 'NONE', #632, #5422 ) ;
#10362 = EDGE_LOOP ( 'NONE', ( #16505, #9765, #10539, #12209, #7407 ) ) ;
#10363 = DIRECTION ( 'NONE',  ( -0.000000000000000000, -0.000000000000000000, -1.000000000000000000 ) ) ;
#10364 = CARTESIAN_POINT ( 'NONE',  ( 20.00000000000000000, 3.000000000000004441, 1.000000000000000000 ) ) ;
#10365 = LINE ( 'NONE', #6913, #14642 ) ;
#10366 = CARTESIAN_POINT ( 'NONE',  ( 13.37499999999998224, -20.24999999999998934, 4.166666666666636765 ) ) ;
#10367 = STYLED_ITEM ( 'NONE', ( #299 ), #4794 ) ;
#10368 = CARTESIAN_POINT ( 'NONE',  ( 0.3749999999999968914, 0.000000000000000000, 1.000000000000000000 ) ) ;
#10369 = CARTESIAN_POINT ( 'NONE',  ( 3.321934647848983957, -9.834888441627915867, 2.750161776669472591 ) ) ;
#10370 = AXIS2_PLACEMENT_3D ( 'NONE', #11721, #19896, #10158 ) ;
#10371 = ADVANCED_FACE ( 'NONE', ( #15766 ), #6055, .T. ) ;
#10372 = CARTESIAN_POINT ( 'NONE',  ( 10.38119784648305810, -14.00000000000000000, 2.000000000000000000 ) ) ;
#10373 = CARTESIAN_POINT ( 'NONE',  ( -12.62499999999998224, -19.49999999999998934, 4.291666666666699825 ) ) ;
#10374 = LINE ( 'NONE', #9289, #8858 ) ;
#10375 = CARTESIAN_POINT ( 'NONE',  ( 12.52780858231679595, -23.72900456129165647, 4.275561207030568411 ) ) ;
#10376 = CARTESIAN_POINT ( 'NONE',  ( -13.41834698511420676, -18.81097725173551893, 6.252442769197418926 ) ) ;
#10377 = PLANE ( 'NONE',  #5697 ) ;
#10378 = EDGE_CURVE ( 'NONE', #1315, #7476, #1544, .T. ) ;
#10379 = CARTESIAN_POINT ( 'NONE',  ( 6.527808582316795949, -22.97900456129165647, 3.964901035250747885 ) ) ;
#10380 = EDGE_CURVE ( 'NONE', #16077, #13777, #17541, .T. ) ;
#10381 = CARTESIAN_POINT ( 'NONE',  ( 4.284691417683176518, -23.77099543870834353, 4.174186261275252718 ) ) ;
#10382 = CARTESIAN_POINT ( 'NONE',  ( -11.87155858231679417, -20.24999999999999289, 3.449312527122348371 ) ) ;
#10383 = DIRECTION ( 'NONE',  ( -1.000000000000000000, 0.000000000000000000, 0.000000000000000000 ) ) ;
#10384 = ORIENTED_EDGE ( 'NONE', *, *, #7312, .T. ) ;
#10385 = CARTESIAN_POINT ( 'NONE',  ( 12.66024186180961308, -19.22028597861421417, 6.258173329156003106 ) ) ;
#10386 = CARTESIAN_POINT ( 'NONE',  ( 13.07121011584135672, 3.033610849983475521, 5.236678440007632496 ) ) ;
#10387 = LINE ( 'NONE', #12052, #1663 ) ;
#10388 = VECTOR ( 'NONE', #11765, 1000.000000000000000 ) ;
#10389 = ORIENTED_EDGE ( 'NONE', *, *, #9611, .T. ) ;
#10390 = VECTOR ( 'NONE', #8618, 1000.000000000000000 ) ;
#10391 = VECTOR ( 'NONE', #13909, 1000.000000000000000 ) ;
#10392 = VERTEX_POINT ( 'NONE', #14091 ) ;
#10393 = DIRECTION ( 'NONE',  ( 0.000000000000000000, -1.000000000000000000, 0.000000000000000000 ) ) ;
#10394 = CARTESIAN_POINT ( 'NONE',  ( -13.49999999999998401, -24.47992105705875332, 12.00000000000000000 ) ) ;
#10395 = DIRECTION ( 'NONE',  ( 0.4999999999999947820, 0.8660254037844417052, -0.000000000000000000 ) ) ;
#10396 = EDGE_CURVE ( 'NONE', #18054, #3979, #19026, .T. ) ;
#10397 = DIRECTION ( 'NONE',  ( 1.000000000000000000, 0.000000000000000000, 0.000000000000000000 ) ) ;
#10398 = CARTESIAN_POINT ( 'NONE',  ( 1.407845757905374695, -9.864917468222230923, 2.372643865078341019 ) ) ;
#10399 = DIRECTION ( 'NONE',  ( 1.000000000000000000, 0.000000000000000000, 0.000000000000000000 ) ) ;
#10400 = FACE_OUTER_BOUND ( 'NONE', #10447, .T. ) ;
#10401 = VECTOR ( 'NONE', #2337, 1000.000000000000000 ) ;
#10402 = DIRECTION ( 'NONE',  ( -0.000000000000000000, 1.000000000000000000, -0.000000000000000000 ) ) ;
#10403 = CARTESIAN_POINT ( 'NONE',  ( -8.402808582316794173, -22.77556120703056308, 1.770995438708339975 ) ) ;
#10404 = CARTESIAN_POINT ( 'NONE',  ( -2.887553741010006281, -10.84643174835951207, 2.067331322690557638 ) ) ;
#10405 = ORIENTED_EDGE ( 'NONE', *, *, #5858, .T. ) ;
#10406 = CARTESIAN_POINT ( 'NONE',  ( -13.37500003877585186, -19.49999804181952712, 4.520055687292853008 ) ) ;
#10407 = CARTESIAN_POINT ( 'NONE',  ( -4.717959273841178636, -21.72818306014730183, 5.243595146365860771 ) ) ;
#10408 = CARTESIAN_POINT ( 'NONE',  ( 9.434058582316795949, -23.73192549717337130, 5.303608408759367343 ) ) ;
#10409 = CARTESIAN_POINT ( 'NONE',  ( -11.59719141768317741, -22.46490103525075810, 4.479004561291653808 ) ) ;
#10410 = ORIENTED_EDGE ( 'NONE', *, *, #12211, .T. ) ;
#10411 = CARTESIAN_POINT ( 'NONE',  ( 13.85593616229004610, 4.037276195647738319, 5.992122970672676630 ) ) ;
#10412 = CARTESIAN_POINT ( 'NONE',  ( 13.50000000000000178, 5.000000000000047962, 4.000000000000000000 ) ) ;
#10413 = ORIENTED_EDGE ( 'NONE', *, *, #8488, .T. ) ;
#10414 = ADVANCED_FACE ( 'NONE', ( #5942 ), #18819, .T. ) ;
#10415 = ORIENTED_EDGE ( 'NONE', *, *, #8284, .F. ) ;
#10416 = DIRECTION ( 'NONE',  ( 0.000000000000000000, -1.000000000000000000, 0.000000000000000000 ) ) ;
#10417 = AXIS2_PLACEMENT_3D ( 'NONE', #10762, #20189, #6056 ) ;
#10418 = EDGE_LOOP ( 'NONE', ( #11442, #12438, #14904, #7205 ) ) ;
#10419 = CARTESIAN_POINT ( 'NONE',  ( -13.39107665282975645, -19.43812903209671461, 5.476542851584349947 ) ) ;
#10420 = VECTOR ( 'NONE', #18616, 1000.000000000000000 ) ;
#10421 = VECTOR ( 'NONE', #16275, 1000.000000000000000 ) ;
#10422 = EDGE_LOOP ( 'NONE', ( #7659, #10493, #2201, #19188, #2721, #4725 ) ) ;
#10423 = LINE ( 'NONE', #16793, #12911 ) ;
#10424 = CARTESIAN_POINT ( 'NONE',  ( 0.000000000000000000, 11.64110105645932691, 10.00000000000000000 ) ) ;
#10425 = EDGE_CURVE ( 'NONE', #7379, #8351, #17442, .T. ) ;
#10426 = EDGE_CURVE ( 'NONE', #19461, #2483, #9495, .T. ) ;
#10427 = CARTESIAN_POINT ( 'NONE',  ( 11.49178095869207006, 4.999999999999999112, 0.000000000000000000 ) ) ;
#10428 = CARTESIAN_POINT ( 'NONE',  ( 1.337453470010121714, -8.364917468222230923, 2.372643865078341019 ) ) ;
#10429 = CARTESIAN_POINT ( 'NONE',  ( -8.309058582316792396, -23.27327832286945153, 2.298404588716537411 ) ) ;
#10430 = CARTESIAN_POINT ( 'NONE',  ( 13.87005939078915873, 4.000499234880882327, 6.742989431566016378 ) ) ;
#10431 = LINE ( 'NONE', #8648, #12969 ) ;
#10432 = CARTESIAN_POINT ( 'NONE',  ( 5.222191417683178294, -20.27099543870833998, 4.275561207030583510 ) ) ;
#10433 = CARTESIAN_POINT ( 'NONE',  ( -12.62499979224180180, -20.25001049178813162, 4.458178821399696012 ) ) ;
#10434 = CARTESIAN_POINT ( 'NONE',  ( -8.409691417683177406, -21.63647391050456648, 4.520995438708348857 ) ) ;
#10435 = AXIS2_PLACEMENT_3D ( 'NONE', #9561, #6537, #1922 ) ;
#10436 = CARTESIAN_POINT ( 'NONE',  ( -9.534691417683177406, -19.47900456129164581, 2.515153566944927199 ) ) ;
#10437 = VERTEX_POINT ( 'NONE', #18713 ) ;
#10438 = CARTESIAN_POINT ( 'NONE',  ( 12.62599452815238443, -19.44977632830967806, 4.656396506304353977 ) ) ;
#10439 = CARTESIAN_POINT ( 'NONE',  ( -13.12529397354238192, 5.014845663890295846, 4.166666666666765551 ) ) ;
#10440 = ORIENTED_EDGE ( 'NONE', *, *, #2878, .F. ) ;
#10441 = ADVANCED_FACE ( 'NONE', ( #4378 ), #10761, .F. ) ;
#10442 = DIRECTION ( 'NONE',  ( 0.4999999999999949485, -0.8660254037844415942, 0.000000000000000000 ) ) ;
#10443 = DIRECTION ( 'NONE',  ( 0.000000000000000000, 0.000000000000000000, 1.000000000000000000 ) ) ;
#10444 =( BOUNDED_CURVE ( )  B_SPLINE_CURVE ( 3, ( #5025, #17790, #5226, #426 ),
 .UNSPECIFIED., .F., .T. ) 
 B_SPLINE_CURVE_WITH_KNOTS ( ( 4, 4 ),
 ( 0.2500000000000000000, 0.5000000000000000000 ),
 .UNSPECIFIED. ) 
 CURVE ( )  GEOMETRIC_REPRESENTATION_ITEM ( )  RATIONAL_B_SPLINE_CURVE ( ( 0.4833790284681487304, 0.4833790284681486193, 0.6445053712908659360, 0.9667580569362994591 ) ) 
 REPRESENTATION_ITEM ( '' )  );
#10445 = VERTEX_POINT ( 'NONE', #2911 ) ;
#10446 = CONTEXT_DEPENDENT_SHAPE_REPRESENTATION ( #14015, #17520 ) ;
#10447 = EDGE_LOOP ( 'NONE', ( #1549, #15920, #6168, #9436 ) ) ;
#10448 = EDGE_LOOP ( 'NONE', ( #2275, #19118, #1233, #267, #8819, #1096, #14007, #19221, #3414 ) ) ;
#10449 = LINE ( 'NONE', #7724, #14308 ) ;
#10450 = AXIS2_PLACEMENT_3D ( 'NONE', #8183, #6609, #12978 ) ;
#10451 = CARTESIAN_POINT ( 'NONE',  ( -20.00000000000000000, -6.000000000000000000, 2.000000000000000000 ) ) ;
#10452 = ADVANCED_FACE ( 'NONE', ( #15663 ), #1347, .T. ) ;
#10453 = CARTESIAN_POINT ( 'NONE',  ( -2.768424032093183662, -10.00067216410020166, 1.850123365707658785 ) ) ;
#10454 = CARTESIAN_POINT ( 'NONE',  ( 0.000000000000000000, 4.999999999999999112, 0.000000000000000000 ) ) ;
#10455 = CARTESIAN_POINT ( 'NONE',  ( 12.00000000000000178, -18.50000000000000355, 4.000000000000000000 ) ) ;
#10456 = LINE ( 'NONE', #13476, #14695 ) ;
#10457 = CARTESIAN_POINT ( 'NONE',  ( 11.03469141768317741, -19.47900456129164581, 2.515153566944927199 ) ) ;
#10458 = CARTESIAN_POINT ( 'NONE',  ( -12.91308523408712183, -5.701695678577235249, 5.798858176249892082 ) ) ;
#10459 = CARTESIAN_POINT ( 'NONE',  ( -9.159691417683175629, -22.98484643305507191, 0.9790045612916508100 ) ) ;
#10460 = ORIENTED_EDGE ( 'NONE', *, *, #11530, .T. ) ;
#10461 = CARTESIAN_POINT ( 'NONE',  ( -11.74178095869206828, 9.000000000000001776, 1.000000000000000000 ) ) ;
#10462 = CARTESIAN_POINT ( 'NONE',  ( 27.50000000000000711, 4.999999999999999112, 1.000000000000000000 ) ) ;
#10463 = CARTESIAN_POINT ( 'NONE',  ( -13.87486364728600208, 4.243114187942282456, 6.725269602253773016 ) ) ;
#10464 = AXIS2_PLACEMENT_3D ( 'NONE', #20206, #12235, #18628 ) ;
#10465 = EDGE_CURVE ( 'NONE', #13688, #6649, #278, .T. ) ;
#10466 = CARTESIAN_POINT ( 'NONE',  ( 12.15280858231679595, -21.22443879296942626, 5.229004561291659137 ) ) ;
#10467 = DIRECTION ( 'NONE',  ( 1.000000000000000000, 0.000000000000000000, -0.000000000000000000 ) ) ;
#10468 = EDGE_LOOP ( 'NONE', ( #202, #13663, #476, #894 ) ) ;
#10469 = ORIENTED_EDGE ( 'NONE', *, *, #2217, .T. ) ;
#10470 = CARTESIAN_POINT ( 'NONE',  ( 13.85593616229004610, 4.037276195647738319, 5.992122970672676630 ) ) ;
#10471 = FACE_OUTER_BOUND ( 'NONE', #240, .T. ) ;
#10472 = ORIENTED_EDGE ( 'NONE', *, *, #11522, .F. ) ;
#10473 = CARTESIAN_POINT ( 'NONE',  ( 4.750698171653723989, 0.000000000000000000, 0.000000000000000000 ) ) ;
#10474 = CARTESIAN_POINT ( 'NONE',  ( 15.00000000000001421, -17.49999999999999645, 1.000000000000000000 ) ) ;
#10475 = CARTESIAN_POINT ( 'NONE',  ( -6.313547257480587760, 16.00000000000000000, 1.000000000000000000 ) ) ;
#10476 = LINE ( 'NONE', #16942, #12924 ) ;
#10477 = FACE_OUTER_BOUND ( 'NONE', #20717, .T. ) ;
#10478 = CARTESIAN_POINT ( 'NONE',  ( 1.731569788986178304, -8.364930642962441709, 1.622647248614820015 ) ) ;
#10479 = FACE_OUTER_BOUND ( 'NONE', #20655, .T. ) ;
#10480 = CARTESIAN_POINT ( 'NONE',  ( -13.12529397354238192, 5.014845663890295846, 4.791666666666685614 ) ) ;
#10481 = DIRECTION ( 'NONE',  ( 1.000000000000000000, 0.000000000000000000, 0.000000000000000000 ) ) ;
#10482 = CARTESIAN_POINT ( 'NONE',  ( -13.38795836133016870, -20.34560275282643005, 5.879540349057044146 ) ) ;
#10483 = LINE ( 'NONE', #5563, #4035 ) ;
#10484 = CARTESIAN_POINT ( 'NONE',  ( 11.40280858231679417, -22.77556120703056308, 1.770995438708339975 ) ) ;
#10485 = CARTESIAN_POINT ( 'NONE',  ( 5.972191417683179182, -23.72900456129165292, 2.724438792969417822 ) ) ;
#10486 = CARTESIAN_POINT ( 'NONE',  ( -12.24655858231679240, -21.94931252712234482, 5.250000000000000888 ) ) ;
#10487 = ORIENTED_EDGE ( 'NONE', *, *, #16771, .T. ) ;
#10488 = CARTESIAN_POINT ( 'NONE',  ( 13.02352923685845631, -0.8742735386340954040, 6.652704579156702991 ) ) ;
#10489 = CARTESIAN_POINT ( 'NONE',  ( 13.08080186171710224, 3.517994016715657146, 5.247095106674282583 ) ) ;
#10490 = DIRECTION ( 'NONE',  ( -1.000000000000000000, -0.000000000000000000, -0.000000000000000000 ) ) ;
#10491 = ORIENTED_EDGE ( 'NONE', *, *, #9784, .F. ) ;
#10492 = EDGE_CURVE ( 'NONE', #4793, #19224, #2652, .T. ) ;
#10493 = ORIENTED_EDGE ( 'NONE', *, *, #6171, .T. ) ;
#10494 = LINE ( 'NONE', #15291, #8123 ) ;
#10495 = AXIS2_PLACEMENT_3D ( 'NONE', #18997, #17731, #8215 ) ;
#10496 = CARTESIAN_POINT ( 'NONE',  ( -12.64511805349267526, -19.23403829861753422, 5.507852591554869726 ) ) ;
#10497 = CARTESIAN_POINT ( 'NONE',  ( -17.05017143803810242, 4.999999999999999112, 1.000000000000000000 ) ) ;
#10498 = DIRECTION ( 'NONE',  ( -0.1736481776669295540, 0.9848077530122082424, 0.000000000000000000 ) ) ;
#10499 = CARTESIAN_POINT ( 'NONE',  ( 0.9854920305337622199, -9.864917468222230923, 2.372643865078341019 ) ) ;
#10500 = DIRECTION ( 'NONE',  ( -0.000000000000000000, -0.000000000000000000, -1.000000000000000000 ) ) ;
#10501 = DIRECTION ( 'NONE',  ( 0.000000000000000000, -0.000000000000000000, 1.000000000000000000 ) ) ;
#10502 = LINE ( 'NONE', #7262, #8647 ) ;
#10503 = CARTESIAN_POINT ( 'NONE',  ( -11.21530858231679595, -24.52099543870834708, 2.515153566944913432 ) ) ;
#10504 = CARTESIAN_POINT ( 'NONE',  ( -2.742252025265078608, -15.06657917462210605, 2.958534504914692942 ) ) ;
#10505 = EDGE_LOOP ( 'NONE', ( #3184, #17155 ) ) ;
#10506 = CARTESIAN_POINT ( 'NONE',  ( -13.45643611822145225, -15.38747602984844853, 4.825999963382285429 ) ) ;
#10507 = LINE ( 'NONE', #14150, #16400 ) ;
#10508 = CARTESIAN_POINT ( 'NONE',  ( 9.722191417683177406, -19.52099543870834353, 4.586221378810406257 ) ) ;
#10509 = CARTESIAN_POINT ( 'NONE',  ( -10.65969141768317741, -22.36352608949543352, 2.479004561291652031 ) ) ;
#10510 = VERTEX_POINT ( 'NONE', #3623 ) ;
#10511 = CARTESIAN_POINT ( 'NONE',  ( 13.39902456816392906, -19.03675930772010361, 5.497554699623231400 ) ) ;
#10512 = CARTESIAN_POINT ( 'NONE',  ( -0.000000000000000000, 11.64110105645932691, 0.000000000000000000 ) ) ;
#10513 = VERTEX_POINT ( 'NONE', #3527 ) ;
#10514 = ORIENTED_EDGE ( 'NONE', *, *, #3222, .F. ) ;
#10515 = CARTESIAN_POINT ( 'NONE',  ( 27.50000000000000711, 4.999999999999999112, 1.000000000000000000 ) ) ;
#10516 = EDGE_CURVE ( 'NONE', #14721, #7382, #490, .T. ) ;
#10517 = ORIENTED_EDGE ( 'NONE', *, *, #5845, .T. ) ;
#10518 = CARTESIAN_POINT ( 'NONE',  ( -13.85163507668220539, 3.820071372449974412, 5.989091157956555556 ) ) ;
#10519 = CIRCLE ( 'NONE', #18539, 2.999999999999999112 ) ;
#10520 = EDGE_CURVE ( 'NONE', #17919, #13894, #16190, .T. ) ;
#10521 = EDGE_CURVE ( 'NONE', #1742, #3392, #8337, .T. ) ;
#10522 = EDGE_LOOP ( 'NONE', ( #13098, #6952, #9967, #16012 ) ) ;
#10523 = CARTESIAN_POINT ( 'NONE',  ( -3.497260319564023057, 0.000000000000000000, 1.000000000000000000 ) ) ;
#10524 = FACE_OUTER_BOUND ( 'NONE', #8771, .T. ) ;
#10525 = DIRECTION ( 'NONE',  ( 1.000000000000000000, 0.000000000000000000, -0.000000000000000000 ) ) ;
#10526 = CARTESIAN_POINT ( 'NONE',  ( 1.548630333695928618, -8.364917468222230923, 2.372643865078341019 ) ) ;
#10527 = CARTESIAN_POINT ( 'NONE',  ( 27.44203811574919882, 0.000000000000000000, 1.000000000000000000 ) ) ;
#10528 = CARTESIAN_POINT ( 'NONE',  ( 12.62500000000002132, -21.00000000000274269, 4.083333333315724012 ) ) ;
#10529 = CARTESIAN_POINT ( 'NONE',  ( 0.000000000000000000, 4.999999999999999112, 0.000000000000000000 ) ) ;
#10530 = LINE ( 'NONE', #18798, #10041 ) ;
#10531 = CARTESIAN_POINT ( 'NONE',  ( -20.92243175760212637, 9.000000000000001776, 1.000000000000000000 ) ) ;
#10532 = CARTESIAN_POINT ( 'NONE',  ( 10.09719141768317741, -22.46490103525075810, 4.479004561291653808 ) ) ;
#10533 = CARTESIAN_POINT ( 'NONE',  ( -12.63249216759192350, -19.87164553660301536, 5.297612231341934041 ) ) ;
#10534 = CARTESIAN_POINT ( 'NONE',  ( -7.003441417683177406, -22.05068747287766229, 4.499999999999999112 ) ) ;
#10535 = CARTESIAN_POINT ( 'NONE',  ( -10.75344141768317741, -21.94931252712233061, 0.9999999999999978906 ) ) ;
#10536 = ORIENTED_EDGE ( 'NONE', *, *, #1538, .T. ) ;
#10537 = CARTESIAN_POINT ( 'NONE',  ( 13.12503131243110843, 5.001581277770153378, 5.166347330538456184 ) ) ;
#10538 = CARTESIAN_POINT ( 'NONE',  ( -13.12529380813666435, 5.014837310896125722, 5.033295791462342628 ) ) ;
#10539 = ORIENTED_EDGE ( 'NONE', *, *, #2066, .F. ) ;
#10540 = LINE ( 'NONE', #2583, #15630 ) ;
#10541 = ADVANCED_FACE ( 'NONE', ( #6871 ), #5195, .F. ) ;
#10542 = DIRECTION ( 'NONE',  ( -0.000000000000000000, 0.000000000000000000, -1.000000000000000000 ) ) ;
#10543 = CIRCLE ( 'NONE', #16212, 10.00000000000000000 ) ;
#10544 = ORIENTED_EDGE ( 'NONE', *, *, #1338, .F. ) ;
#10545 = ORIENTED_EDGE ( 'NONE', *, *, #10465, .F. ) ;
#10546 = EDGE_LOOP ( 'NONE', ( #9596, #17750, #16100, #3272 ) ) ;
#10547 = DIRECTION ( 'NONE',  ( 1.000000000000000000, 0.000000000000000000, 0.000000000000000000 ) ) ;
#10548 = FACE_OUTER_BOUND ( 'NONE', #4471, .T. ) ;
#10549 = CARTESIAN_POINT ( 'NONE',  ( -2.044552395631970665, -10.13052631352519306, 1.690857522621936226 ) ) ;
#10550 = PLANE ( 'NONE',  #16379 ) ;
#10551 = CARTESIAN_POINT ( 'NONE',  ( 0.000000000000000000, 16.00000000000000000, 1.000000000000000000 ) ) ;
#10552 = EDGE_CURVE ( 'NONE', #6507, #5903, #13238, .T. ) ;
#10553 = DIRECTION ( 'NONE',  ( -0.000000000000000000, -0.000000000000000000, -1.000000000000000000 ) ) ;
#10554 = CARTESIAN_POINT ( 'NONE',  ( 6.809058582316796837, -23.80360840875935935, 1.768074502826626260 ) ) ;
#10555 = CARTESIAN_POINT ( 'NONE',  ( -12.66369984131459070, -18.29565801360988075, 5.528024842915327142 ) ) ;
#10556 = CARTESIAN_POINT ( 'NONE',  ( -7.190941417683177406, -23.80360840875937001, 5.231925497173365081 ) ) ;
#10557 =( BOUNDED_CURVE ( )  B_SPLINE_CURVE ( 2, ( #3171, #19184, #6417, #6201, #8090, #15916, #4733, #11319, #14455, #12883, #6301, #19286, #17703, #11121, #3375, #18969, #19076, #4838, #9338, #7876, #4530, #4625, #11018, #9754, #10914, #15714, #17491, #14235, #16139, #1397, #9545, #1593, #3070, #12570, #17388, #9446, #7973, #15817, #14346, #30, #3683, #18011, #8401, #11732, #6726, #14768, #1904, #13193, #17810, #10067, #16440, #14867, #445, #7033, #2012, #14661, #8191, #19691, #16632, #542, #16537, #3476, #17907, #5245, #6824, #5354, #19591, #14557, #10265, #11526, #8287, #19806, #2212, #16238, #18124, #11622, #2115, #8594, #11833, #3885, #6617, #5148, #6921, #14964, #8497, #13290, #342, #3574, #3790, #9953, #13093, #645, #16338, #19496, #9853 ),
 .UNSPECIFIED., .F., .F. ) 
 B_SPLINE_CURVE_WITH_KNOTS ( ( 3, 2, 2, 2, 2, 2, 2, 2, 2, 2, 2, 2, 2, 2, 2, 2, 2, 2, 2, 2, 2, 2, 2, 2, 2, 2, 2, 2, 2, 2, 2, 2, 2, 2, 2, 2, 2, 2, 2, 2, 2, 2, 2, 2, 2, 2, 2, 3 ),
 ( 0.000000000000000000, 0.02083333333333333218, 0.04166666666666666435, 0.06250000000000000000, 0.08333333333333332871, 0.1041666666666666713, 0.1250000000000000000, 0.1458333333333333426, 0.1666666666666666574, 0.1875000000000000000, 0.2083333333333333426, 0.2291666666666666574, 0.2500000000000000000, 0.2708333333333333148, 0.2916666666666666852, 0.3124999999999999445, 0.3333333333333333148, 0.3541666666666666852, 0.3750000000000000000, 0.3958333333333333148, 0.4166666666666666852, 0.4375000000000000555, 0.4583333333333333148, 0.4791666666666666852, 0.5000000000000000000, 0.5208333333333333703, 0.5416666666666666297, 0.5625000000000000000, 0.5833333333333333703, 0.6041666666666666297, 0.6249999999999998890, 0.6458333333333333703, 0.6666666666666666297, 0.6875000000000000000, 0.7083333333333333703, 0.7291666666666666297, 0.7500000000000000000, 0.7708333333333333703, 0.7916666666666666297, 0.8125000000000000000, 0.8333333333333333703, 0.8541666666666666297, 0.8750000000000001110, 0.8958333333333333703, 0.9166666666666666297, 0.9375000000000000000, 0.9583333333333333703, 0.9650437087885355147 ),
 .UNSPECIFIED. ) 
 CURVE ( )  GEOMETRIC_REPRESENTATION_ITEM ( )  RATIONAL_B_SPLINE_CURVE ( ( 1.000000000000000000, 0.9238795325112867385, 1.000000000000000000, 0.9238795325112867385, 1.000000000000000000, 0.9238795325112867385, 1.000000000000000000, 0.9238795325112867385, 1.000000000000000000, 0.9238795325112867385, 1.000000000000000000, 0.9238795325112867385, 1.000000000000000000, 0.9238795325112867385, 1.000000000000000000, 0.9238795325112867385, 1.000000000000000000, 0.9238795325112867385, 1.000000000000000000, 0.9238795325112867385, 1.000000000000000000, 0.9238795325112867385, 1.000000000000000000, 0.9238795325112867385, 1.000000000000000000, 0.9238795325112867385, 1.000000000000000000, 0.9238795325112867385, 1.000000000000000000, 0.9238795325112867385, 1.000000000000000000, 0.9238795325112867385, 1.000000000000000000, 0.9238795325112867385, 1.000000000000000000, 0.9238795325112867385, 1.000000000000000000, 0.9238795325112867385, 1.000000000000000000, 0.9238795325112867385, 1.000000000000000000, 0.9238795325112867385, 1.000000000000000000, 0.9238795325112867385, 1.000000000000000000, 0.9238795325112867385, 1.000000000000000000, 0.9238795325112867385, 1.000000000000000000, 0.9238795325112867385, 1.000000000000000000, 0.9238795325112867385, 1.000000000000000000, 0.9238795325112867385, 1.000000000000000000, 0.9238795325112867385, 1.000000000000000000, 0.9238795325112867385, 1.000000000000000000, 0.9238795325112867385, 1.000000000000000000, 0.9238795325112867385, 1.000000000000000000, 0.9238795325112867385, 1.000000000000000000, 0.9238795325112867385, 1.000000000000000000, 0.9238795325112867385, 1.000000000000000000, 0.9238795325112867385, 1.000000000000000000, 0.9238795325112867385, 1.000000000000000000, 0.9238795325112867385, 1.000000000000000000, 0.9238795325112867385, 1.000000000000000000, 0.9238795325112867385, 1.000000000000000000, 0.9238795325112867385, 1.000000000000000000, 0.9238795325112867385, 1.000000000000000000, 0.9238795325112867385, 1.000000000000000000, 0.9238795325112867385, 1.000000000000000000, 0.9238795325112867385, 1.000000000000000000, 0.9238795325112867385, 1.000000000000000000, 0.9238795325112867385, 1.000000000000000000, 0.9754817479996107377, 0.9667580569362973497 ) ) 
 REPRESENTATION_ITEM ( '' )  );
#10558 = ORIENTED_EDGE ( 'NONE', *, *, #6560, .T. ) ;
#10559 = DIRECTION ( 'NONE',  ( -0.7071067811865475727, 0.000000000000000000, -0.7071067811865475727 ) ) ;
#10560 = LINE ( 'NONE', #2495, #15428 ) ;
#10561 = CARTESIAN_POINT ( 'NONE',  ( -13.37500027835944039, -20.99998594284889464, 4.544258551573043370 ) ) ;
#10562 = AXIS2_PLACEMENT_3D ( 'NONE', #2068, #285, #6875 ) ;
#10563 = CARTESIAN_POINT ( 'NONE',  ( 10.09030858231679595, -21.32581373872472597, 1.729004561291657582 ) ) ;
#10564 = EDGE_CURVE ( 'NONE', #9890, #7068, #10007, .T. ) ;
#10565 = DIRECTION ( 'NONE',  ( 0.000000000000000000, 1.000000000000000000, 0.000000000000000000 ) ) ;
#10566 = EDGE_LOOP ( 'NONE', ( #20565, #7278, #13560, #17898 ) ) ;
#10567 = EDGE_CURVE ( 'NONE', #2846, #14519, #16385, .T. ) ;
#10568 = ORIENTED_EDGE ( 'NONE', *, *, #10682, .T. ) ;
#10569 = CARTESIAN_POINT ( 'NONE',  ( 13.42074492158312715, -18.68988146005270679, 6.255046935864005064 ) ) ;
#10570 = DIRECTION ( 'NONE',  ( -0.000000000000000000, -0.000000000000000000, -1.000000000000000000 ) ) ;
#10571 = ORIENTED_EDGE ( 'NONE', *, *, #20314, .F. ) ;
#10572 = CARTESIAN_POINT ( 'NONE',  ( 0.000000000000000000, 4.999999999999999112, 1.000000000000000000 ) ) ;
#10573 = VERTEX_POINT ( 'NONE', #19332 ) ;
#10574 = FACE_OUTER_BOUND ( 'NONE', #11960, .T. ) ;
#10575 = DIRECTION ( 'NONE',  ( -0.000000000000000000, -0.000000000000000000, -1.000000000000000000 ) ) ;
#10576 = CARTESIAN_POINT ( 'NONE',  ( -14.00000000000000000, 0.000000000000000000, 1.000000000000000000 ) ) ;
#10577 = CARTESIAN_POINT ( 'NONE',  ( 2.808565762442263303, -10.28561894962424716, 1.923303392614186924 ) ) ;
#10578 = EDGE_CURVE ( 'NONE', #2072, #3209, #2063, .T. ) ;
#10579 = CARTESIAN_POINT ( 'NONE',  ( 2.786182376113650605, -10.12667130264514626, 1.882483419865550900 ) ) ;
#10580 = CARTESIAN_POINT ( 'NONE',  ( -13.09560264576187905, 4.265433610975056133, 4.791666666666684726 ) ) ;
#10581 = DIRECTION ( 'NONE',  ( -1.000000000000000000, 4.625929269271486111E-15, 0.000000000000000000 ) ) ;
#10582 = CARTESIAN_POINT ( 'NONE',  ( -13.40322194933353828, -19.57479155865495457, 6.214283636730510096 ) ) ;
#10583 = LINE ( 'NONE', #16751, #14708 ) ;
#10584 = CARTESIAN_POINT ( 'NONE',  ( 12.52780858231679595, -23.72900456129165647, 4.275561207030568411 ) ) ;
#10585 = CARTESIAN_POINT ( 'NONE',  ( 6.065941417683177406, -23.20159541128344927, 2.226721677130534705 ) ) ;
#10586 = CARTESIAN_POINT ( 'NONE',  ( -10.18405858231679417, -20.79840458871652942, 2.226721677130544030 ) ) ;
#10587 = ORIENTED_EDGE ( 'NONE', *, *, #16308, .T. ) ;
#10588 = CARTESIAN_POINT ( 'NONE',  ( 12.67794853492974561, -16.82609898603114118, 4.809595106674325216 ) ) ;
#10589 = CARTESIAN_POINT ( 'NONE',  ( 0.6250000000000005551, 10.00000000000000000, 0.000000000000000000 ) ) ;
#10590 = ORIENTED_EDGE ( 'NONE', *, *, #3150, .F. ) ;
#10591 = ORIENTED_EDGE ( 'NONE', *, *, #15811, .F. ) ;
#10592 = CARTESIAN_POINT ( 'NONE',  ( -0.1250000000000035805, 4.999999999999999112, 0.000000000000000000 ) ) ;
#10593 = CARTESIAN_POINT ( 'NONE',  ( -13.05696142222617695, 1.564051822406025583, 5.955108176248398166 ) ) ;
#10594 = CARTESIAN_POINT ( 'NONE',  ( -2.645259258103298983, -10.28229522185712241, 2.672449792925449596 ) ) ;
#10595 = CARTESIAN_POINT ( 'NONE',  ( -13.80667376788930056, 1.549525278393783179, 5.940263032956496048 ) ) ;
#10596 = DIRECTION ( 'NONE',  ( -1.000000000000000000, 0.000000000000000000, 0.000000000000000000 ) ) ;
#10597 = LINE ( 'NONE', #15405, #13208 ) ;
#10598 = DIRECTION ( 'NONE',  ( 0.000000000000000000, 1.000000000000000000, 0.000000000000000000 ) ) ;
#10599 = CARTESIAN_POINT ( 'NONE',  ( -19.48630159782011262, 9.000000000000001776, 0.000000000000000000 ) ) ;
#10600 = LINE ( 'NONE', #18659, #19351 ) ;
#10601 = CARTESIAN_POINT ( 'NONE',  ( -9.152808582316795949, -20.91377862118960351, 5.979004561291660913 ) ) ;
#10602 = CARTESIAN_POINT ( 'NONE',  ( -1.798207051321043304, -8.367281747657623114, 1.623251059268568053 ) ) ;
#10603 = ORIENTED_EDGE ( 'NONE', *, *, #19526, .F. ) ;
#10604 = AXIS2_PLACEMENT_3D ( 'NONE', #3034, #17459, #11279 ) ;
#10605 = CARTESIAN_POINT ( 'NONE',  ( -13.84501469867711698, 4.235742283194553259, 4.916666666666649199 ) ) ;
#10606 = LINE ( 'NONE', #2969, #16060 ) ;
#10607 = CARTESIAN_POINT ( 'NONE',  ( 9.909691417683175629, -21.01515356694492098, 6.020995438708349745 ) ) ;
#10608 = CARTESIAN_POINT ( 'NONE',  ( -8.034691417683175629, -20.97900456129164581, 3.136473910504570917 ) ) ;
#10609 = ORIENTED_EDGE ( 'NONE', *, *, #19153, .F. ) ;
#10610 = ADVANCED_FACE ( 'NONE', ( #19233 ), #18194, .T. ) ;
#10611 = CARTESIAN_POINT ( 'NONE',  ( 13.80667376788930056, 1.549525278393783179, 5.940263032956496048 ) ) ;
#10612 = CARTESIAN_POINT ( 'NONE',  ( 0.000000000000000000, 16.00000000000000000, 1.000000000000000000 ) ) ;
#10613 = ORIENTED_EDGE ( 'NONE', *, *, #8851, .F. ) ;
#10614 = VERTEX_POINT ( 'NONE', #18455 ) ;
#10615 = CARTESIAN_POINT ( 'NONE',  ( 21.25349085826861995, 0.000000000000000000, 0.000000000000000000 ) ) ;
#10616 = ORIENTED_EDGE ( 'NONE', *, *, #3410, .T. ) ;
#10617 = CARTESIAN_POINT ( 'NONE',  ( -13.87470602645761986, 4.985154336109792972, 4.791666666666685614 ) ) ;
#10618 = LINE ( 'NONE', #15429, #2546 ) ;
#10619 = VERTEX_POINT ( 'NONE', #20448 ) ;
#10620 = DIRECTION ( 'NONE',  ( 1.000000000000000000, 0.000000000000000000, -0.000000000000000000 ) ) ;
#10621 = CIRCLE ( 'NONE', #4946, 10.00000000000000000 ) ;
#10622 = DIRECTION ( 'NONE',  ( 0.000000000000000000, 1.000000000000000000, -0.000000000000000000 ) ) ;
#10623 = CARTESIAN_POINT ( 'NONE',  ( -14.49999999999998579, -21.99999999999999645, 9.999999999999998224 ) ) ;
#10624 = CARTESIAN_POINT ( 'NONE',  ( 3.302240162463773832, -9.695145533921818881, 2.714273006325518711 ) ) ;
#10625 = PLANE ( 'NONE',  #19565 ) ;
#10626 = EDGE_CURVE ( 'NONE', #8919, #6152, #17181, .T. ) ;
#10627 = CARTESIAN_POINT ( 'NONE',  ( 6.183390479346035917, 4.999999999999999112, 0.000000000000000000 ) ) ;
#10628 = DIRECTION ( 'NONE',  ( 1.000000000000000000, 0.000000000000000000, 0.000000000000000000 ) ) ;
#10629 = CARTESIAN_POINT ( 'NONE',  ( 19.23630159782011617, 9.000000000000001776, 1.000000000000000000 ) ) ;
#10630 = CARTESIAN_POINT ( 'NONE',  ( 4.378441417683176518, -23.74999999999999645, 3.449312527122335492 ) ) ;
#10631 = CARTESIAN_POINT ( 'NONE',  ( -12.62515553039088090, -20.24214571525854467, 4.629702272822510345 ) ) ;
#10632 = CARTESIAN_POINT ( 'NONE',  ( -9.152808582316795949, -21.53509896474924901, 4.479004561291659137 ) ) ;
#10633 = CARTESIAN_POINT ( 'NONE',  ( -8.222191417683175629, -19.52099543870834353, 4.586221378810406257 ) ) ;
#10634 = VECTOR ( 'NONE', #17956, 1000.000000000000000 ) ;
#10635 = ORIENTED_EDGE ( 'NONE', *, *, #20017, .F. ) ;
#10636 = EDGE_CURVE ( 'NONE', #20224, #19548, #12262, .T. ) ;
#10637 = CARTESIAN_POINT ( 'NONE',  ( 13.12512971825177033, 5.006550771716304915, 5.133277049491872468 ) ) ;
#10638 = CARTESIAN_POINT ( 'NONE',  ( -13.12463908936614132, 4.981774012991869505, 5.264611377988129171 ) ) ;
#10639 = EDGE_LOOP ( 'NONE', ( #17301, #6603, #2921, #12071 ) ) ;
#10640 = EDGE_CURVE ( 'NONE', #11334, #12338, #15214, .T. ) ;
#10641 = AXIS2_PLACEMENT_3D ( 'NONE', #9582, #11060, #10752 ) ;
#10642 = CARTESIAN_POINT ( 'NONE',  ( 11.00000000000000000, -20.16506350946107418, 5.250000000000000000 ) ) ;
#10643 = FACE_OUTER_BOUND ( 'NONE', #8437, .T. ) ;
#10644 = ORIENTED_EDGE ( 'NONE', *, *, #18634, .T. ) ;
#10645 = CARTESIAN_POINT ( 'NONE',  ( 1.710927537542899612, -9.866086492083725901, 2.372944093759576933 ) ) ;
#10646 = VECTOR ( 'NONE', #17924, 1000.000000000000227 ) ;
#10647 = VERTEX_POINT ( 'NONE', #20233 ) ;
#10648 = LINE ( 'NONE', #4064, #6658 ) ;
#10649 = CARTESIAN_POINT ( 'NONE',  ( 24.62918902992234038, 10.00000000000000000, 1.000000000000000000 ) ) ;
#10650 = VECTOR ( 'NONE', #17836, 1000.000000000000000 ) ;
#10651 = CARTESIAN_POINT ( 'NONE',  ( -0.9854920305337621089, -9.114917468222230923, 1.622643865078341463 ) ) ;
#10652 = LINE ( 'NONE', #13570, #9360 ) ;
#10653 = DIRECTION ( 'NONE',  ( 1.000000000000000000, 0.000000000000000000, 0.000000000000000000 ) ) ;
#10654 = AXIS2_PLACEMENT_3D ( 'NONE', #1138, #17228, #8974 ) ;
#10655 = EDGE_CURVE ( 'NONE', #487, #16591, #12475, .T. ) ;
#10656 = DIRECTION ( 'NONE',  ( -1.000000000000000000, 0.000000000000000000, 0.000000000000000000 ) ) ;
#10657 = CARTESIAN_POINT ( 'NONE',  ( 4.746558582316795061, -21.94931252712234127, 6.000000000000001776 ) ) ;
#10658 = CARTESIAN_POINT ( 'NONE',  ( -13.10756170493883310, 4.119366099410778581, 6.001761809183453700 ) ) ;
#10659 = CARTESIAN_POINT ( 'NONE',  ( -12.53469141768317741, -20.22900456129164581, 2.825813738724747726 ) ) ;
#10660 = VERTEX_POINT ( 'NONE', #14039 ) ;
#10661 = CARTESIAN_POINT ( 'NONE',  ( 12.24655858231679240, -21.94931252712234482, 5.250000000000000888 ) ) ;
#10662 = CARTESIAN_POINT ( 'NONE',  ( -5.433390479346035029, 0.000000000000000000, 0.000000000000000000 ) ) ;
#10663 = CARTESIAN_POINT ( 'NONE',  ( -13.71569110726703045, -3.795099083046435506, 6.575359435862661250 ) ) ;
#10664 = VECTOR ( 'NONE', #1518, 1000.000000000000000 ) ;
#10665 = VECTOR ( 'NONE', #14502, 1000.000000000000000 ) ;
#10666 = CARTESIAN_POINT ( 'NONE',  ( 9.996558582316794173, -22.05068747287764452, 1.749999999999998446 ) ) ;
#10667 = LINE ( 'NONE', #14106, #642 ) ;
#10668 = AXIS2_PLACEMENT_3D ( 'NONE', #19039, #14000, #18933 ) ;
#10669 = ORIENTED_EDGE ( 'NONE', *, *, #13881, .F. ) ;
#10670 = ORIENTED_EDGE ( 'NONE', *, *, #5944, .F. ) ;
#10671 = CARTESIAN_POINT ( 'NONE',  ( 13.79242507427300879, 0.07996625081441015304, 6.658692769197546824 ) ) ;
#10672 = AXIS2_PLACEMENT_3D ( 'NONE', #11569, #18164, #3830 ) ;
#10673 = CARTESIAN_POINT ( 'NONE',  ( 0.000000000000000000, 9.000000000000001776, 1.000000000000000000 ) ) ;
#10674 = ORIENTED_EDGE ( 'NONE', *, *, #6345, .F. ) ;
#10675 = LINE ( 'NONE', #10473, #8793 ) ;
#10676 = ORIENTED_EDGE ( 'NONE', *, *, #1139, .T. ) ;
#10677 = CARTESIAN_POINT ( 'NONE',  ( -8.965308582316794173, -20.22900456129164937, 4.174186261275266929 ) ) ;
#10678 = FACE_OUTER_BOUND ( 'NONE', #3604, .T. ) ;
#10679 = CARTESIAN_POINT ( 'NONE',  ( -19.48630159782011262, 0.000000000000000000, 1.000000000000000000 ) ) ;
#10680 = VECTOR ( 'NONE', #13854, 1000.000000000000000 ) ;
#10681 = CARTESIAN_POINT ( 'NONE',  ( 3.462011766956747394, -14.92507028461178287, 3.114807177791267812 ) ) ;
#10682 = EDGE_CURVE ( 'NONE', #6243, #19704, #10597, .T. ) ;
#10683 = VECTOR ( 'NONE', #17068, 1000.000000000000000 ) ;
#10684 = EDGE_CURVE ( 'NONE', #18061, #8657, #1396, .T. ) ;
#10685 = CARTESIAN_POINT ( 'NONE',  ( -14.49999999999998401, -25.49999999999999645, 4.000000000000000000 ) ) ;
#10686 = CARTESIAN_POINT ( 'NONE',  ( -13.37523871602689596, -19.48794484064217514, 4.577160611493482634 ) ) ;
#10687 = CARTESIAN_POINT ( 'NONE',  ( 12.90280858231679773, -22.77556120703056308, 1.770995438708339975 ) ) ;
#10688 = CARTESIAN_POINT ( 'NONE',  ( -13.87470602645415063, 4.985154336109792972, 3.333333333332063830 ) ) ;
#10689 = CIRCLE ( 'NONE', #12693, 1.000000000000002665 ) ;
#10690 = LINE ( 'NONE', #18639, #17053 ) ;
#10691 = CARTESIAN_POINT ( 'NONE',  ( 9.902808582316794173, -22.77556120703056308, 1.770995438708339975 ) ) ;
#10692 = CARTESIAN_POINT ( 'NONE',  ( 12.62844141768317741, -20.99999999999999645, 3.550687472877664952 ) ) ;
#10693 = CARTESIAN_POINT ( 'NONE',  ( -5.402808582316794173, -22.77556120703056308, 1.770995438708339975 ) ) ;
#10694 = ORIENTED_EDGE ( 'NONE', *, *, #13595, .F. ) ;
#10695 = CARTESIAN_POINT ( 'NONE',  ( 13.09560264575884503, 4.265433610975056133, 3.333333333333364568 ) ) ;
#10696 = VECTOR ( 'NONE', #11695, 1000.000000000000000 ) ;
#10697 = CARTESIAN_POINT ( 'NONE',  ( 2.687849085826861995, 0.000000000000000000, 0.000000000000000000 ) ) ;
#10698 = VERTEX_POINT ( 'NONE', #1189 ) ;
#10699 = ADVANCED_FACE ( 'NONE', ( #18656 ), #17080, .T. ) ;
#10700 = ORIENTED_EDGE ( 'NONE', *, *, #3525, .T. ) ;
#10701 = LINE ( 'NONE', #12467, #757 ) ;
#10702 = AXIS2_PLACEMENT_3D ( 'NONE', #16262, #11648, #671 ) ;
#10703 = CARTESIAN_POINT ( 'NONE',  ( -12.62524871736568954, -20.23743977303344010, 4.661898514667671023 ) ) ;
#10704 = CARTESIAN_POINT ( 'NONE',  ( -2.436080212393455735, -9.483920418190111334, 2.467411194204634839 ) ) ;
#10705 = CARTESIAN_POINT ( 'NONE',  ( -13.49014615398506045, -14.43511922376608680, 5.596513032956658584 ) ) ;
#10706 = LINE ( 'NONE', #17079, #18356 ) ;
#10707 = DIRECTION ( 'NONE',  ( 1.000000000000000000, 6.938893903907222067E-15, 0.000000000000000000 ) ) ;
#10708 = PLANE ( 'NONE',  #464 ) ;
#10709 = DIRECTION ( 'NONE',  ( 0.000000000000000000, 1.000000000000000000, -0.000000000000000000 ) ) ;
#10710 = DIRECTION ( 'NONE',  ( 0.000000000000000000, -0.000000000000000000, 1.000000000000000000 ) ) ;
#10711 = CARTESIAN_POINT ( 'NONE',  ( -4.687312169500632564, -21.51559725698341197, 5.182386163300427562 ) ) ;
#10712 = CARTESIAN_POINT ( 'NONE',  ( -1.652577328807104839, -9.114908150887895744, 1.622641472200749835 ) ) ;
#10713 = VERTEX_POINT ( 'NONE', #15605 ) ;
#10714 = CARTESIAN_POINT ( 'NONE',  ( -13.38800411018677572, -19.59329243556743805, 5.436267741224407146 ) ) ;
#10715 = MECHANICAL_DESIGN_GEOMETRIC_PRESENTATION_REPRESENTATION (  '', ( #1680 ), #2036 ) ;
#10716 = DIRECTION ( 'NONE',  ( -0.000000000000000000, -0.000000000000000000, -1.000000000000000000 ) ) ;
#10717 = VECTOR ( 'NONE', #19313, 1000.000000000000000 ) ;
#10718 = CARTESIAN_POINT ( 'NONE',  ( 10.84719141768317741, -20.91377862118959285, 1.020995438708345082 ) ) ;
#10719 = CARTESIAN_POINT ( 'NONE',  ( -9.347191417683177406, -21.53509896474923835, 2.520995438708346192 ) ) ;
#10720 = ORIENTED_EDGE ( 'NONE', *, *, #17706, .T. ) ;
#10721 = CARTESIAN_POINT ( 'NONE',  ( 13.42793873098995938, -18.32659408500397191, 6.262859435864284841 ) ) ;
#10722 = CARTESIAN_POINT ( 'NONE',  ( 12.62499999999998579, -20.24999999999999289, 3.146526952850934755 ) ) ;
#10723 = EDGE_LOOP ( 'NONE', ( #12792, #17244, #1027, #2614 ) ) ;
#10724 = VERTEX_POINT ( 'NONE', #14234 ) ;
#10725 = EDGE_CURVE ( 'NONE', #3875, #2724, #18868, .T. ) ;
#10726 = CARTESIAN_POINT ( 'NONE',  ( 12.25209451496117197, 11.64110105645932691, 0.000000000000000000 ) ) ;
#10727 = VERTEX_POINT ( 'NONE', #4529 ) ;
#10728 = CARTESIAN_POINT ( 'NONE',  ( -13.84264281492353987, 3.365962153638767607, 5.979325532956542233 ) ) ;
#10729 = CARTESIAN_POINT ( 'NONE',  ( 1.655860418491166941, -9.114909740826840689, 2.372641880528837621 ) ) ;
#10730 = AXIS2_PLACEMENT_3D ( 'NONE', #2939, #18950, #4605 ) ;
#10731 = ORIENTED_EDGE ( 'NONE', *, *, #17986, .F. ) ;
#10732 = CARTESIAN_POINT ( 'NONE',  ( -7.499999999999999112, -25.49999999999999645, 4.000000000000000000 ) ) ;
#10733 = FACE_OUTER_BOUND ( 'NONE', #12332, .T. ) ;
#10734 = AXIS2_PLACEMENT_3D ( 'NONE', #15508, #8833, #15407 ) ;
#10735 = VECTOR ( 'NONE', #3068, 1000.000000000000000 ) ;
#10736 = DIRECTION ( 'NONE',  ( 2.312964634635731617E-15, -1.000000000000000000, 0.000000000000000000 ) ) ;
#10737 = CARTESIAN_POINT ( 'NONE',  ( 0.9854920305337622199, -8.364917468222230923, 1.622643865078341907 ) ) ;
#10738 = CARTESIAN_POINT ( 'NONE',  ( 0.000000000000000000, 9.000000000000001776, 0.000000000000000000 ) ) ;
#10739 = CARTESIAN_POINT ( 'NONE',  ( 13.10756170493883310, 4.119366099410778581, 6.001761809183453700 ) ) ;
#10740 = PLANE ( 'NONE',  #18312 ) ;
#10741 = CARTESIAN_POINT ( 'NONE',  ( -15.00000000000000000, 3.000000000000000000, 2.000000000000000000 ) ) ;
#10742 = CARTESIAN_POINT ( 'NONE',  ( 21.17243175760212637, 0.000000000000000000, 0.000000000000000000 ) ) ;
#10743 = CARTESIAN_POINT ( 'NONE',  ( 5.315941417683176518, -21.32873467460645145, 4.242948236979555254 ) ) ;
#10744 = CARTESIAN_POINT ( 'NONE',  ( -12.65410809543883985, -18.78004118034163739, 5.517608176248461227 ) ) ;
#10745 = CARTESIAN_POINT ( 'NONE',  ( -12.05905858231679595, -21.25705176302045274, 4.171265325393551215 ) ) ;
#10746 = CARTESIAN_POINT ( 'NONE',  ( -10.28469141768317741, -24.52099543870834708, 4.484846433055073689 ) ) ;
#10747 = ORIENTED_EDGE ( 'NONE', *, *, #7610, .T. ) ;
#10748 = CARTESIAN_POINT ( 'NONE',  ( 13.05202662408965075, 2.064844516520778939, 5.215845106673912213 ) ) ;
#10749 = DIRECTION ( 'NONE',  ( 0.8660254037844415942, 0.4999999999999949485, -0.000000000000000000 ) ) ;
#10750 = EDGE_LOOP ( 'NONE', ( #19434, #14397, #501, #2078 ) ) ;
#10751 = VECTOR ( 'NONE', #13681, 1000.000000000000000 ) ;
#10752 = DIRECTION ( 'NONE',  ( 0.000000000000000000, 0.000000000000000000, 1.000000000000000000 ) ) ;
#10753 = EDGE_LOOP ( 'NONE', ( #10756, #12562, #2080, #5392 ) ) ;
#10754 = CARTESIAN_POINT ( 'NONE',  ( 1.939860967060266672, -10.52577007527361808, 2.542364016426418516 ) ) ;
#10755 = EDGE_CURVE ( 'NONE', #3444, #1636, #6200, .T. ) ;
#10756 = ORIENTED_EDGE ( 'NONE', *, *, #17673, .F. ) ;
#10757 = CARTESIAN_POINT ( 'NONE',  ( 8.119520639128047890, 4.999999999999999112, 0.000000000000000000 ) ) ;
#10758 = CARTESIAN_POINT ( 'NONE',  ( 0.000000000000000000, 11.64110105645932691, 10.00000000000000000 ) ) ;
#10759 = EDGE_CURVE ( 'NONE', #16591, #17, #9445, .T. ) ;
#10760 = CARTESIAN_POINT ( 'NONE',  ( -2.155282726790247239, -12.05525952636828357, 2.935167462089139256 ) ) ;
#10761 = PLANE ( 'NONE',  #11040 ) ;
#10762 = CARTESIAN_POINT ( 'NONE',  ( 2.693754455098655409, -10.04853567022903782, 2.237415670251142519 ) ) ;
#10763 = ADVANCED_FACE ( 'NONE', ( #7567 ), #12164, .T. ) ;
#10764 = AXIS2_PLACEMENT_3D ( 'NONE', #9779, #18998, #14579 ) ;
#10765 = DIRECTION ( 'NONE',  ( 1.000000000000000000, 0.000000000000000000, 0.000000000000000000 ) ) ;
#10766 = LINE ( 'NONE', #3501, #11353 ) ;
#10767 = CARTESIAN_POINT ( 'NONE',  ( 8.034691417683175629, -19.47900456129164581, 2.515153566944927199 ) ) ;
#10768 = CARTESIAN_POINT ( 'NONE',  ( -13.12529397354238192, 5.014845663890295846, 3.000000000000000000 ) ) ;
#10769 = CARTESIAN_POINT ( 'NONE',  ( -7.378441417683176518, -23.74999999999999645, 3.449312527122335492 ) ) ;
#10770 = ORIENTED_EDGE ( 'NONE', *, *, #3150, .T. ) ;
#10771 = CARTESIAN_POINT ( 'NONE',  ( 6.809058582316794173, -23.27327832286945153, 2.298404588716537411 ) ) ;
#10772 = DIRECTION ( 'NONE',  ( -3.469446951953619119E-16, 1.000000000000000000, 0.000000000000000000 ) ) ;
#10773 = CARTESIAN_POINT ( 'NONE',  ( -13.42793873098995938, -18.32659408500397191, 6.262859435864284841 ) ) ;
#10774 = VERTEX_POINT ( 'NONE', #17387 ) ;
#10775 = VECTOR ( 'NONE', #10416, 1000.000000000000000 ) ;
#10776 = CARTESIAN_POINT ( 'NONE',  ( 10.37155858231679417, -20.24999999999999289, 3.449312527122348371 ) ) ;
#10777 = CARTESIAN_POINT ( 'NONE',  ( -3.497260319564023057, 9.000000000000001776, 1.000000000000000000 ) ) ;
#10778 = ORIENTED_EDGE ( 'NONE', *, *, #13307, .T. ) ;
#10779 = ORIENTED_EDGE ( 'NONE', *, *, #6596, .F. ) ;
#10780 = CARTESIAN_POINT ( 'NONE',  ( 13.45671396861735403, -16.87344458480707843, 6.294109435864141844 ) ) ;
#10781 = DIRECTION ( 'NONE',  ( 1.000000000000000000, 0.000000000000000000, 0.000000000000000000 ) ) ;
#10782 = ORIENTED_EDGE ( 'NONE', *, *, #6489, .T. ) ;
#10783 = VECTOR ( 'NONE', #12898, 1000.000000000000000 ) ;
#10784 = EDGE_CURVE ( 'NONE', #2075, #2607, #7779, .T. ) ;
#10785 = DIRECTION ( 'NONE',  ( -0.9908228861781570584, 0.1309180808328758994, -0.03362237850931586169 ) ) ;
#10786 = ORIENTED_EDGE ( 'NONE', *, *, #2352, .T. ) ;
#10787 = CARTESIAN_POINT ( 'NONE',  ( -11.12155858231679417, -23.74999999999999645, 3.550687472877651629 ) ) ;
#10788 = CARTESIAN_POINT ( 'NONE',  ( 13.87470586348985258, 4.985146106231644225, 5.033049509202228933 ) ) ;
#10789 = EDGE_CURVE ( 'NONE', #12772, #14282, #2178, .T. ) ;
#10790 = DIRECTION ( 'NONE',  ( 0.000000000000000000, 1.000000000000000000, 0.000000000000000000 ) ) ;
#10791 = CARTESIAN_POINT ( 'NONE',  ( 1.754777266914451461, -9.116337928146160507, 1.623008667563337726 ) ) ;
#10792 = EDGE_CURVE ( 'NONE', #20520, #1608, #12569, .T. ) ;
#10793 = LINE ( 'NONE', #20109, #16403 ) ;
#10794 = CARTESIAN_POINT ( 'NONE',  ( -13.37680511754115287, -19.40884156416817774, 4.692171866446762429 ) ) ;
#10795 = LINE ( 'NONE', #5774, #16411 ) ;
#10796 = CARTESIAN_POINT ( 'NONE',  ( -13.60059015675642513, -9.607697083824668027, 6.450359435862663027 ) ) ;
#10797 = AXIS2_PLACEMENT_3D ( 'NONE', #5260, #16762, #462 ) ;
#10798 = DIRECTION ( 'NONE',  ( -0.000000000000000000, -0.000000000000000000, -1.000000000000000000 ) ) ;
#10799 = CARTESIAN_POINT ( 'NONE',  ( 5.590308582316795949, -21.63647391050454871, 2.479004561291657804 ) ) ;
#10800 = CARTESIAN_POINT ( 'NONE',  ( 10.00344141768317741, -22.05068747287766229, 4.499999999999999112 ) ) ;
#10801 = CARTESIAN_POINT ( 'NONE',  ( -10.56594141768317741, -23.20159541128344927, 2.226721677130534705 ) ) ;
#10802 = ORIENTED_EDGE ( 'NONE', *, *, #5914, .T. ) ;
#10803 = CARTESIAN_POINT ( 'NONE',  ( 13.37503747255156306, -19.49810763614315690, 4.531249681074674740 ) ) ;
#10804 = CARTESIAN_POINT ( 'NONE',  ( -2.589709240944451096, -9.559844081062008669, 1.736909907557668165 ) ) ;
#10805 = ORIENTED_EDGE ( 'NONE', *, *, #9518, .F. ) ;
#10806 = ADVANCED_FACE ( 'NONE', ( #9035 ), #6274, .T. ) ;
#10807 = ORIENTED_EDGE ( 'NONE', *, *, #16617, .F. ) ;
#10808 = ADVANCED_BREP_SHAPE_REPRESENTATION ( '', ( #17970, #18039 ), #15032 ) ;
#10809 = LINE ( 'NONE', #12058, #3428 ) ;
#10810 = VECTOR ( 'NONE', #18423, 1000.000000000000000 ) ;
#10811 = CARTESIAN_POINT ( 'NONE',  ( -12.64323021897839006, -19.32937394158751943, 5.504219675487169283 ) ) ;
#10812 = CARTESIAN_POINT ( 'NONE',  ( -1.824488249492779879, -9.124319963227819130, 2.375058613629473570 ) ) ;
#10813 = CARTESIAN_POINT ( 'NONE',  ( -13.87470602645761986, 4.985154336109792972, 4.583333333333296622 ) ) ;
#10814 = CARTESIAN_POINT ( 'NONE',  ( -13.00000000000000355, 6.123233995736754943E-17, 2.000000000000000000 ) ) ;
#10815 = CARTESIAN_POINT ( 'NONE',  ( -12.62499999999998224, -20.24999999999998934, 4.291666666666698937 ) ) ;
#10816 = CARTESIAN_POINT ( 'NONE',  ( 0.000000000000000000, 4.999999999999999112, 0.000000000000000000 ) ) ;
#10817 = FACE_OUTER_BOUND ( 'NONE', #17297, .T. ) ;
#10818 = EDGE_CURVE ( 'NONE', #11436, #9041, #3125, .T. ) ;
#10819 = LINE ( 'NONE', #5895, #1632 ) ;
#10820 = CARTESIAN_POINT ( 'NONE',  ( -7.746558582316795949, -21.94931252712234127, 6.000000000000001776 ) ) ;
#10821 = CARTESIAN_POINT ( 'NONE',  ( -2.226467333542268445, -8.440126719678968215, 1.641959103308203716 ) ) ;
#10822 = AXIS2_PLACEMENT_3D ( 'NONE', #6081, #20210, #4406 ) ;
#10823 = ORIENTED_EDGE ( 'NONE', *, *, #9073, .T. ) ;
#10824 = CARTESIAN_POINT ( 'NONE',  ( -13.37499999998404121, -20.24999999996810729, 2.793053905886972998 ) ) ;
#10825 = LINE ( 'NONE', #13738, #3708 ) ;
#10826 = CARTESIAN_POINT ( 'NONE',  ( 10.37844141768317741, -24.50000000000000000, 3.449312527122335048 ) ) ;
#10827 = CARTESIAN_POINT ( 'NONE',  ( -5.784691417683178294, -23.02099543870834353, 3.863526089495429972 ) ) ;
#10828 = ORIENTED_EDGE ( 'NONE', *, *, #5658, .F. ) ;
#10829 = CARTESIAN_POINT ( 'NONE',  ( 13.37923893525309715, -20.78593376972237650, 5.366589449429977954 ) ) ;
#10830 = CARTESIAN_POINT ( 'NONE',  ( 26.04469207716615031, 0.000000000000000000, 1.000000000000000000 ) ) ;
#10831 = ORIENTED_EDGE ( 'NONE', *, *, #5398, .F. ) ;
#10832 = ORIENTED_EDGE ( 'NONE', *, *, #8984, .F. ) ;
#10833 = CARTESIAN_POINT ( 'NONE',  ( -11.74178095869206828, 9.000000000000001776, 0.000000000000000000 ) ) ;
#10834 = ADVANCED_FACE ( 'NONE', ( #15871 ), #20506, .F. ) ;
#10835 = VERTEX_POINT ( 'NONE', #19030 ) ;
#10836 = EDGE_CURVE ( 'NONE', #3725, #1633, #14097, .T. ) ;
#10837 = CARTESIAN_POINT ( 'NONE',  ( -13.85403523778986390, 3.941279508358651817, 5.991705257707216958 ) ) ;
#10838 = VECTOR ( 'NONE', #18350, 1000.000000000000000 ) ;
#10839 = CARTESIAN_POINT ( 'NONE',  ( 1.337453470010121714, -9.114917468222230923, 2.372643865078341019 ) ) ;
#10840 = ORIENTED_EDGE ( 'NONE', *, *, #13403, .T. ) ;
#10841 = DIRECTION ( 'NONE',  ( 0.000000000000000000, 1.000000000000000000, 0.000000000000000000 ) ) ;
#10842 = DIRECTION ( 'NONE',  ( 1.000000000000000000, -2.312964634635752916E-15, 0.000000000000000000 ) ) ;
#10843 = FACE_OUTER_BOUND ( 'NONE', #8248, .T. ) ;
#10844 = CARTESIAN_POINT ( 'NONE',  ( 2.801385037117921861, -10.23463596792102415, 1.910209944425432349 ) ) ;
#10845 = LINE ( 'NONE', #12401, #5965 ) ;
#10846 = CARTESIAN_POINT ( 'NONE',  ( 13.12119116326504908, 4.807653744879115010, 5.626470997801169105 ) ) ;
#10847 = EDGE_CURVE ( 'NONE', #14996, #10231, #15771, .T. ) ;
#10848 = FACE_OUTER_BOUND ( 'NONE', #18594, .T. ) ;
#10849 = CARTESIAN_POINT ( 'NONE',  ( 0.000000000000000000, 10.00000000000000000, 1.000000000000000000 ) ) ;
#10850 = DIRECTION ( 'NONE',  ( 0.000000000000000000, 0.000000000000000000, 1.000000000000000000 ) ) ;
#10851 = CARTESIAN_POINT ( 'NONE',  ( 4.378441417683176518, -22.99999999999999645, 3.449312527122335048 ) ) ;
#10852 = CARTESIAN_POINT ( 'NONE',  ( -13.00900269284621302, -0.8578640112522492034, 5.903024842915844062 ) ) ;
#10853 = CARTESIAN_POINT ( 'NONE',  ( -8.496558582316795949, -22.05068747287764452, 2.499999999999999112 ) ) ;
#10854 = CARTESIAN_POINT ( 'NONE',  ( -4.003441417683175629, -22.05068747287766229, 6.000000000000001776 ) ) ;
#10855 = VERTEX_POINT ( 'NONE', #1547 ) ;
#10856 = CARTESIAN_POINT ( 'NONE',  ( 13.37499999999998401, -19.49999999999998934, 3.666666666666654084 ) ) ;
#10857 = CARTESIAN_POINT ( 'NONE',  ( 2.311130159782011972, 0.000000000000000000, 0.000000000000000000 ) ) ;
#10858 = ORIENTED_EDGE ( 'NONE', *, *, #20374, .T. ) ;
#10859 = DIRECTION ( 'NONE',  ( 0.000000000000000000, -1.000000000000000000, 0.000000000000000000 ) ) ;
#10860 = EDGE_LOOP ( 'NONE', ( #9310, #20349, #4312, #7918, #3313 ) ) ;
#10861 = CARTESIAN_POINT ( 'NONE',  ( 1.982945319006538032, -10.83166796549307520, 2.620924705558935308 ) ) ;
#10862 = MANIFOLD_SOLID_BREP ( 'Chamfer1', #2975 ) ;
#10863 = ORIENTED_EDGE ( 'NONE', *, *, #6668, .T. ) ;
#10864 = CARTESIAN_POINT ( 'NONE',  ( 6.183390479346035917, 0.000000000000000000, 0.000000000000000000 ) ) ;
#10865 = CARTESIAN_POINT ( 'NONE',  ( -30.00000000000000000, 10.00000000000000000, 0.000000000000000000 ) ) ;
#10866 = CARTESIAN_POINT ( 'NONE',  ( -1.337453470010121714, -9.114917468222230923, 1.622643865078341463 ) ) ;
#10867 = DIRECTION ( 'NONE',  ( 0.000000000000000000, 0.000000000000000000, 1.000000000000000000 ) ) ;
#10868 = CARTESIAN_POINT ( 'NONE',  ( -20.00349085826861995, 0.000000000000000000, 0.000000000000000000 ) ) ;
#10869 = CARTESIAN_POINT ( 'NONE',  ( -3.500698171653725765, 0.000000000000000000, 1.000000000000000000 ) ) ;
#10870 = CARTESIAN_POINT ( 'NONE',  ( 7.284691417683176518, -24.52099543870834708, 4.484846433055073689 ) ) ;
#10871 = LINE ( 'NONE', #17340, #1185 ) ;
#10872 = CARTESIAN_POINT ( 'NONE',  ( -11.12844141768317741, -20.24999999999999289, 3.550687472877664952 ) ) ;
#10873 = EDGE_CURVE ( 'NONE', #5957, #8181, #10871, .T. ) ;
#10874 = ORIENTED_EDGE ( 'NONE', *, *, #7611, .T. ) ;
#10875 = CARTESIAN_POINT ( 'NONE',  ( 8.777808582316792396, -20.27099543870833642, 2.724438792969431589 ) ) ;
#10876 = FACE_OUTER_BOUND ( 'NONE', #17744, .T. ) ;
#10877 = CARTESIAN_POINT ( 'NONE',  ( -12.62499999998404299, -20.99999999996810729, 2.793053905886972998 ) ) ;
#10878 = ORIENTED_EDGE ( 'NONE', *, *, #15279, .T. ) ;
#10879 = CARTESIAN_POINT ( 'NONE',  ( 8.871558582316794173, -20.24999999999999289, 3.449312527122348371 ) ) ;
#10880 = CARTESIAN_POINT ( 'NONE',  ( -14.50000000000000000, -21.00000000000000355, 1.000000000000000000 ) ) ;
#10881 = ORIENTED_EDGE ( 'NONE', *, *, #1074, .T. ) ;
#10882 = CARTESIAN_POINT ( 'NONE',  ( 13.86316420010827777, 3.652292105464413297, 6.735515685864076119 ) ) ;
#10883 = LINE ( 'NONE', #20203, #13139 ) ;
#10884 = VECTOR ( 'NONE', #3069, 1000.000000000000000 ) ;
#10885 = VERTEX_POINT ( 'NONE', #17447 ) ;
#10886 = CARTESIAN_POINT ( 'NONE',  ( 27.52582389412042474, 4.853545418763153485, 1.000000000000000000 ) ) ;
#10887 = ORIENTED_EDGE ( 'NONE', *, *, #5501, .T. ) ;
#10888 = CARTESIAN_POINT ( 'NONE',  ( -10.65280858231679240, -21.22443879296942626, 5.229004561291659137 ) ) ;
#10889 = DIRECTION ( 'NONE',  ( 0.000000000000000000, 1.000000000000000000, 0.000000000000000000 ) ) ;
#10890 = CARTESIAN_POINT ( 'NONE',  ( 21.25349085826861995, 10.00000000000000000, 0.000000000000000000 ) ) ;
#10891 = CARTESIAN_POINT ( 'NONE',  ( 1.619022621591186928, -8.364917468222230923, 1.622643865078341907 ) ) ;
#10892 = LINE ( 'NONE', #3348, #3713 ) ;
#10893 = CARTESIAN_POINT ( 'NONE',  ( -13.37847682517167947, -19.32442032882675775, 4.733786629989340078 ) ) ;
#10894 = CARTESIAN_POINT ( 'NONE',  ( 8.684058582316794173, -20.79840458871652942, 2.226721677130544030 ) ) ;
#10895 = CARTESIAN_POINT ( 'NONE',  ( -13.89730118381875279, 5.376209782841177898, 6.083536567043803522 ) ) ;
#10896 = EDGE_CURVE ( 'NONE', #17122, #15169, #15543, .T. ) ;
#10897 = DIRECTION ( 'NONE',  ( 1.000000000000000000, -1.156482317317871133E-15, 0.000000000000000000 ) ) ;
#10898 = CARTESIAN_POINT ( 'NONE',  ( 5.684058582316794173, -20.79840458871652942, 2.226721677130544030 ) ) ;
#10899 = CARTESIAN_POINT ( 'NONE',  ( 8.128441417683177406, -20.99999999999999645, 3.550687472877664952 ) ) ;
#10900 = CARTESIAN_POINT ( 'NONE',  ( -11.87844141768317563, -23.74999999999999645, 3.449312527122335492 ) ) ;
#10901 = ORIENTED_EDGE ( 'NONE', *, *, #2957, .T. ) ;
#10902 = ADVANCED_FACE ( 'NONE', ( #9291 ), #15666, .T. ) ;
#10903 = CARTESIAN_POINT ( 'NONE',  ( 13.09560264576187905, 4.265433610975056133, 4.666666666666618113 ) ) ;
#10904 = ADVANCED_FACE ( 'NONE', ( #18924 ), #10969, .T. ) ;
#10905 = CARTESIAN_POINT ( 'NONE',  ( -1.548630333695928396, -9.114917468222230923, 1.622643865078341463 ) ) ;
#10906 = ORIENTED_EDGE ( 'NONE', *, *, #471, .T. ) ;
#10907 = VERTEX_POINT ( 'NONE', #7831 ) ;
#10908 = CARTESIAN_POINT ( 'NONE',  ( -3.497260319564023057, 0.000000000000000000, 1.000000000000000000 ) ) ;
#10909 = CARTESIAN_POINT ( 'NONE',  ( -12.62745083560477966, -20.12623280195927933, 5.001038150054709419 ) ) ;
#10910 = CARTESIAN_POINT ( 'NONE',  ( -1.407845757905374695, -9.114917468222230923, 2.372643865078341019 ) ) ;
#10911 = CARTESIAN_POINT ( 'NONE',  ( -13.87470602645761986, 4.985154336109792972, 4.333333333333382775 ) ) ;
#10912 = DIRECTION ( 'NONE',  ( 0.000000000000000000, 0.000000000000000000, 1.000000000000000000 ) ) ;
#10913 = DIRECTION ( 'NONE',  ( 0.000000000000000000, -0.000000000000000000, 1.000000000000000000 ) ) ;
#10914 = CARTESIAN_POINT ( 'NONE',  ( 11.12155858231679417, -23.74999999999999645, 3.550687472877651629 ) ) ;
#10915 = CARTESIAN_POINT ( 'NONE',  ( 0.000000000000000000, 9.000000000000001776, 0.000000000000000000 ) ) ;
#10916 = CARTESIAN_POINT ( 'NONE',  ( 12.62499999999998401, -20.24999999999998934, 2.439580858552613751 ) ) ;
#10917 = EDGE_CURVE ( 'NONE', #7723, #10445, #18903, .T. ) ;
#10918 = CARTESIAN_POINT ( 'NONE',  ( -13.27780858231679417, -19.52099543870833642, 2.413778621189609286 ) ) ;
#10919 = CARTESIAN_POINT ( 'NONE',  ( -1.896776615114361908, -10.21987218505477024, 2.463803327293850209 ) ) ;
#10920 = ORIENTED_EDGE ( 'NONE', *, *, #20472, .F. ) ;
#10921 = CARTESIAN_POINT ( 'NONE',  ( -13.84501469867711698, 4.235742283194553259, 4.791666666666684726 ) ) ;
#10922 = CARTESIAN_POINT ( 'NONE',  ( 7.619520639128047002, 4.999999999999999112, 0.000000000000000000 ) ) ;
#10923 = CARTESIAN_POINT ( 'NONE',  ( 10.65969141768317741, -22.98484643305507191, 0.9790045612916508100 ) ) ;
#10924 = CARTESIAN_POINT ( 'NONE',  ( -4.847191417683177406, -21.53509896474923835, 2.520995438708346192 ) ) ;
#10925 = ORIENTED_EDGE ( 'NONE', *, *, #15607, .T. ) ;
#10926 = CARTESIAN_POINT ( 'NONE',  ( 13.37499999999998224, -21.00000000000006395, 4.416666666666682062 ) ) ;
#10927 = CARTESIAN_POINT ( 'NONE',  ( 12.62524871736568954, -20.23743977303344010, 4.661898514667671023 ) ) ;
#10928 = ORIENTED_EDGE ( 'NONE', *, *, #4405, .F. ) ;
#10929 = ORIENTED_EDGE ( 'NONE', *, *, #16926, .T. ) ;
#10930 = CARTESIAN_POINT ( 'NONE',  ( -0.000000000000000000, 10.00000000000000000, 0.000000000000000000 ) ) ;
#10931 = ORIENTED_EDGE ( 'NONE', *, *, #936, .F. ) ;
#10932 = CARTESIAN_POINT ( 'NONE',  ( -13.85980676119184629, 4.232741440188380722, 5.965367510457697975 ) ) ;
#10933 = CARTESIAN_POINT ( 'NONE',  ( 2.367358971471363649, -9.400572650371021410, 2.446005822389718087 ) ) ;
#10934 = EDGE_LOOP ( 'NONE', ( #15685, #8744, #19735, #5185, #399, #1485 ) ) ;
#10935 = DIRECTION ( 'NONE',  ( 0.000000000000000000, 1.000000000000000000, 0.000000000000000000 ) ) ;
#10936 = CARTESIAN_POINT ( 'NONE',  ( 3.162271481458107658, -13.95306990448253437, 3.615178062515473911 ) ) ;
#10937 = PLANE ( 'NONE',  #15673 ) ;
#10938 = CARTESIAN_POINT ( 'NONE',  ( 1.906542528716098417, -8.376716462152538512, 1.625674082428238298 ) ) ;
#10939 = DIRECTION ( 'NONE',  ( -8.673617379884045333E-17, 1.000000000000000000, 0.000000000000000000 ) ) ;
#10940 = CARTESIAN_POINT ( 'NONE',  ( 13.12270769621861355, 4.884238659038159902, 5.513847264053151065 ) ) ;
#10941 = ADVANCED_FACE ( 'NONE', ( #6252, #14404, #18718 ), #18072, .F. ) ;
#10942 = CARTESIAN_POINT ( 'NONE',  ( -30.00000000000000000, 3.000000000000000000, 0.000000000000000000 ) ) ;
#10943 = FACE_OUTER_BOUND ( 'NONE', #19523, .T. ) ;
#10944 = ADVANCED_FACE ( 'NONE', ( #5103 ), #1859, .T. ) ;
#10945 = DIRECTION ( 'NONE',  ( 0.000000000000000000, 1.000000000000000000, -0.000000000000000000 ) ) ;
#10946 = CARTESIAN_POINT ( 'NONE',  ( 7.003441417683177406, -22.05068747287766229, 4.499999999999999112 ) ) ;
#10947 = CARTESIAN_POINT ( 'NONE',  ( -13.06655316810189227, 2.048434989138931961, 5.965524842914772030 ) ) ;
#10948 = CARTESIAN_POINT ( 'NONE',  ( -7.934058582316796837, -22.67126532539354855, 4.242948236979545484 ) ) ;
#10949 = CARTESIAN_POINT ( 'NONE',  ( -4.097191417683177406, -23.08622137881040359, 5.979004561291654696 ) ) ;
#10950 = EDGE_CURVE ( 'NONE', #9451, #5395, #187, .T. ) ;
#10951 = EDGE_LOOP ( 'NONE', ( #18471, #1769 ) ) ;
#10952 = CARTESIAN_POINT ( 'NONE',  ( 12.93692567357942202, -3.747753484270499591, 5.090845106672844622 ) ) ;
#10953 = CARTESIAN_POINT ( 'NONE',  ( -18.98630159782011262, 9.000000000000001776, 1.000000000000000000 ) ) ;
#10954 = ORIENTED_EDGE ( 'NONE', *, *, #14474, .T. ) ;
#10955 = CARTESIAN_POINT ( 'NONE',  ( 16.37779268661489596, 10.00000000000000000, 0.000000000000000000 ) ) ;
#10956 = ORIENTED_EDGE ( 'NONE', *, *, #6030, .F. ) ;
#10957 = CARTESIAN_POINT ( 'NONE',  ( 0.2815691515810352374, -9.864917468222230923, 2.372643865078523540 ) ) ;
#10958 = CIRCLE ( 'NONE', #6273, 0.5000000000000000000 ) ;
#10959 = ADVANCED_FACE ( 'NONE', ( #14918 ), #9704, .T. ) ;
#10960 = ORIENTED_EDGE ( 'NONE', *, *, #7138, .T. ) ;
#10961 = CARTESIAN_POINT ( 'NONE',  ( 8.222191417683175629, -20.27099543870833998, 4.275561207030583510 ) ) ;
#10962 = LINE ( 'NONE', #17330, #12650 ) ;
#10963 = CARTESIAN_POINT ( 'NONE',  ( -1.925499516411631973, -10.42380411186744382, 2.516177120048874283 ) ) ;
#10964 = CARTESIAN_POINT ( 'NONE',  ( 9.000000000000000000, -9.999999999999991118, 2.500000000000000000 ) ) ;
#10965 = CARTESIAN_POINT ( 'NONE',  ( 0.000000000000000000, 9.000000000000001776, 0.000000000000000000 ) ) ;
#10966 =( GEOMETRIC_REPRESENTATION_CONTEXT ( 3 ) GLOBAL_UNCERTAINTY_ASSIGNED_CONTEXT ( ( #20125 ) ) GLOBAL_UNIT_ASSIGNED_CONTEXT ( ( #6364, #5101, #19136 ) ) REPRESENTATION_CONTEXT ( 'NONE', 'WORKASPACE' ) );
#10967 = PLANE ( 'NONE',  #944 ) ;
#10968 = CARTESIAN_POINT ( 'NONE',  ( 12.44094141768317741, -20.72672167713052715, 2.298404588716546293 ) ) ;
#10969 = PLANE ( 'NONE',  #7204 ) ;
#10970 = VECTOR ( 'NONE', #17434, 1000.000000000000000 ) ;
#10971 = CARTESIAN_POINT ( 'NONE',  ( -11.03469141768318273, -20.22900456129164581, 2.825813738724747726 ) ) ;
#10972 = ORIENTED_EDGE ( 'NONE', *, *, #6720, .F. ) ;
#10973 = CARTESIAN_POINT ( 'NONE',  ( 6.059058582316793284, -20.72672167713054137, 4.701595411283463477 ) ) ;
#10974 = CARTESIAN_POINT ( 'NONE',  ( 20.00000000000000000, -5.999999999999994671, 2.000000000000000000 ) ) ;
#10975 = CARTESIAN_POINT ( 'NONE',  ( -13.02352923685845631, -0.8742735386340954040, 6.652704579156702991 ) ) ;
#10976 = ORIENTED_EDGE ( 'NONE', *, *, #11571, .T. ) ;
#10977 = CARTESIAN_POINT ( 'NONE',  ( 8.777808582316792396, -20.27099543870833642, 2.724438792969431589 ) ) ;
#10978 = CARTESIAN_POINT ( 'NONE',  ( -11.99999999999999467, -17.50000000000000000, 4.000000000000000000 ) ) ;
#10979 = ORIENTED_EDGE ( 'NONE', *, *, #12986, .T. ) ;
#10980 = CYLINDRICAL_SURFACE ( 'NONE', #10604, 0.2500000000000002220 ) ;
#10981 =( NAMED_UNIT ( * ) PLANE_ANGLE_UNIT ( ) SI_UNIT ( $, .RADIAN. ) );
#10982 = ORIENTED_EDGE ( 'NONE', *, *, #9665, .T. ) ;
#10983 = EDGE_CURVE ( 'NONE', #14522, #19324, #396, .T. ) ;
#10984 = VECTOR ( 'NONE', #11722, 1000.000000000000000 ) ;
#10985 = DIRECTION ( 'NONE',  ( -0.000000000000000000, -0.000000000000000000, -1.000000000000000000 ) ) ;
#10986 = VERTEX_POINT ( 'NONE', #19546 ) ;
#10987 = CARTESIAN_POINT ( 'NONE',  ( -11.77780858231679417, -20.27099543870833642, 2.724438792969431589 ) ) ;
#10988 = CARTESIAN_POINT ( 'NONE',  ( 12.62503117662529739, -20.24842558042254836, 4.565011198945062354 ) ) ;
#10989 = PLANE ( 'NONE',  #180 ) ;
#10990 = CARTESIAN_POINT ( 'NONE',  ( 2.031432063436913182, -10.08997855658269671, 1.680444048616273722 ) ) ;
#10991 = EDGE_CURVE ( 'NONE', #7631, #16247, #19445, .T. ) ;
#10992 = CARTESIAN_POINT ( 'NONE',  ( 8.126396343307449754, 11.64110105645932691, 10.00000000000000000 ) ) ;
#10993 = CARTESIAN_POINT ( 'NONE',  ( -13.07121011584135672, 3.033610849983475521, 5.236678440007632496 ) ) ;
#10994 = VECTOR ( 'NONE', #5720, 1000.000000000000000 ) ;
#10995 = CARTESIAN_POINT ( 'NONE',  ( 6.246558582316794173, -21.94931252712234482, 5.250000000000000888 ) ) ;
#10996 = CARTESIAN_POINT ( 'NONE',  ( -12.64802275499843454, -19.83735087257960927, 6.157588447769994922 ) ) ;
#10997 = VECTOR ( 'NONE', #8354, 1000.000000000000000 ) ;
#10998 = CARTESIAN_POINT ( 'NONE',  ( 0.000000000000000000, 9.000000000000001776, 1.000000000000000000 ) ) ;
#10999 = CARTESIAN_POINT ( 'NONE',  ( 7.090308582316794173, -21.32581373872472597, 1.729004561291657582 ) ) ;
#11000 = AXIS2_PLACEMENT_3D ( 'NONE', #5843, #1032, #15245 ) ;
#11001 = CARTESIAN_POINT ( 'NONE',  ( 5.690941417683177406, -22.74294823697955081, 4.171265325393542334 ) ) ;
#11002 = CARTESIAN_POINT ( 'NONE',  ( -5.965308582316793284, -20.22900456129164937, 4.174186261275266929 ) ) ;
#11003 = ORIENTED_EDGE ( 'NONE', *, *, #6084, .T. ) ;
#11004 = CARTESIAN_POINT ( 'NONE',  ( 13.37500003877585186, -19.49999804181952712, 4.520055687292853008 ) ) ;
#11005 = CARTESIAN_POINT ( 'NONE',  ( -2.309828811027716977, -9.292785183284841821, 1.668323847571005603 ) ) ;
#11006 = ORIENTED_EDGE ( 'NONE', *, *, #17304, .F. ) ;
#11007 = ORIENTED_EDGE ( 'NONE', *, *, #18453, .T. ) ;
#11008 = CARTESIAN_POINT ( 'NONE',  ( 4.750698171653723989, 11.64110105645932691, 0.000000000000000000 ) ) ;
#11009 = VECTOR ( 'NONE', #14165, 1000.000000000000000 ) ;
#11010 = AXIS2_PLACEMENT_3D ( 'NONE', #10424, #2463, #8854 ) ;
#11011 = ADVANCED_FACE ( 'NONE', ( #14607 ), #9907, .T. ) ;
#11012 = PLANE ( 'NONE',  #1245 ) ;
#11013 = AXIS2_PLACEMENT_3D ( 'NONE', #9081, #18499, #6534 ) ;
#11014 = CARTESIAN_POINT ( 'NONE',  ( -1.932703420524435112, -8.381852853175612239, 2.376993210252662969 ) ) ;
#11015 = FACE_OUTER_BOUND ( 'NONE', #7045, .T. ) ;
#11016 = CARTESIAN_POINT ( 'NONE',  ( 2.739050625766161762, -9.875938058683834342, 1.818089155622620412 ) ) ;
#11017 = DIRECTION ( 'NONE',  ( 1.000000000000000000, 0.000000000000000000, 0.000000000000000000 ) ) ;
#11018 = CARTESIAN_POINT ( 'NONE',  ( 11.30905858231679417, -23.27327832286945153, 2.298404588716537411 ) ) ;
#11019 = EDGE_CURVE ( 'NONE', #7736, #8434, #16289, .T. ) ;
#11020 = CARTESIAN_POINT ( 'NONE',  ( 32.65117217603048516, 6.460468870412194420, 1.000000000000000000 ) ) ;
#11021 = CARTESIAN_POINT ( 'NONE',  ( 13.14782865898149034, 5.402847278557675104, 6.092770214907355708 ) ) ;
#11022 = CARTESIAN_POINT ( 'NONE',  ( -6.715308582316796837, -24.52099543870834708, 2.515153566944913432 ) ) ;
#11023 = CARTESIAN_POINT ( 'NONE',  ( -2.196516900615978152, -11.19187256518208784, 1.963432442569047698 ) ) ;
#11024 = ORIENTED_EDGE ( 'NONE', *, *, #1690, .F. ) ;
#11025 = AXIS2_PLACEMENT_3D ( 'NONE', #18094, #19073, #4730 ) ;
#11026 = CARTESIAN_POINT ( 'NONE',  ( -13.39482594849551944, -19.24878960097397140, 5.493002502378098839 ) ) ;
#11027 = DIRECTION ( 'NONE',  ( 0.000000000000000000, -0.9919684228235026158, 0.1264857625231113336 ) ) ;
#11028 = CARTESIAN_POINT ( 'NONE',  ( 6.065941417683177406, -23.73192549717336064, 1.696391591240623331 ) ) ;
#11029 = CARTESIAN_POINT ( 'NONE',  ( -13.27780858231679417, -21.02099543870833998, 3.035098964749253003 ) ) ;
#11030 = ORIENTED_EDGE ( 'NONE', *, *, #6322, .F. ) ;
#11031 = CARTESIAN_POINT ( 'NONE',  ( 13.37543017851028893, -20.97827598523083026, 4.780017688621249761 ) ) ;
#11032 = DIRECTION ( 'NONE',  ( 1.000000000000000000, 0.000000000000000000, 0.000000000000000000 ) ) ;
#11033 = CARTESIAN_POINT ( 'NONE',  ( 9.830951894845298966, -2.500000000000047518, 7.000000000000000000 ) ) ;
#11034 = ORIENTED_EDGE ( 'NONE', *, *, #7074, .T. ) ;
#11035 = VECTOR ( 'NONE', #13265, 1000.000000000000000 ) ;
#11036 = ORIENTED_EDGE ( 'NONE', *, *, #11983, .F. ) ;
#11037 = DIRECTION ( 'NONE',  ( 1.000000000000000000, 0.000000000000000000, 0.000000000000000000 ) ) ;
#11038 = EDGE_CURVE ( 'NONE', #3437, #16270, #11675, .T. ) ;
#11039 = DIRECTION ( 'NONE',  ( 0.000000000000000000, -0.000000000000000000, 1.000000000000000000 ) ) ;
#11040 = AXIS2_PLACEMENT_3D ( 'NONE', #17131, #2810, #15560 ) ;
#11041 = VERTEX_POINT ( 'NONE', #4888 ) ;
#11042 = DIRECTION ( 'NONE',  ( 1.000000000000000000, 0.000000000000000000, 0.000000000000000000 ) ) ;
#11043 = CARTESIAN_POINT ( 'NONE',  ( -14.49999999999998579, -18.49999999999999645, 4.000000000000000000 ) ) ;
#11044 = CARTESIAN_POINT ( 'NONE',  ( -14.99999999999999645, -30.00000000000000711, 1.000000000000000000 ) ) ;
#11045 = CARTESIAN_POINT ( 'NONE',  ( 3.506783328160878010, -9.991161114504492957, 2.040295720924476530 ) ) ;
#11046 = CARTESIAN_POINT ( 'NONE',  ( 3.747260319564023501, 4.999999999999999112, 0.000000000000000000 ) ) ;
#11047 = DIRECTION ( 'NONE',  ( 1.000000000000000000, 0.000000000000000000, 0.000000000000000000 ) ) ;
#11048 = AXIS2_PLACEMENT_3D ( 'NONE', #3981, #18001, #747 ) ;
#11049 = PLANE ( 'NONE',  #17993 ) ;
#11050 = CARTESIAN_POINT ( 'NONE',  ( -13.18405858231679417, -20.79840458871652942, 2.226721677130544030 ) ) ;
#11051 = CARTESIAN_POINT ( 'NONE',  ( -1.904508877737772998, -9.138371295333994837, 2.378667276417936627 ) ) ;
#11052 = CARTESIAN_POINT ( 'NONE',  ( 12.80905858231679417, -22.74294823697954016, 2.828734674606448785 ) ) ;
#11053 = CARTESIAN_POINT ( 'NONE',  ( -13.11514659413808737, 4.502403003978772134, 5.887634658581065494 ) ) ;
#11054 = CARTESIAN_POINT ( 'NONE',  ( -11.21530858231679595, -23.02099543870833998, 3.136473910504556262 ) ) ;
#11055 = CARTESIAN_POINT ( 'NONE',  ( -10.84719141768317563, -21.22443879296941915, 1.770995438708345748 ) ) ;
#11056 = EDGE_LOOP ( 'NONE', ( #14328, #5601, #16034, #7768 ) ) ;
#11057 = CARTESIAN_POINT ( 'NONE',  ( 13.09560264576187905, 4.265433610975056133, 4.916666666666649199 ) ) ;
#11058 = DIRECTION ( 'NONE',  ( 1.000000000000000000, -0.000000000000000000, 0.000000000000000000 ) ) ;
#11059 = EDGE_LOOP ( 'NONE', ( #17097, #11772, #9356, #15473 ) ) ;
#11060 = DIRECTION ( 'NONE',  ( -1.000000000000000000, 0.000000000000000000, 0.000000000000000000 ) ) ;
#11061 = VERTEX_POINT ( 'NONE', #4994 ) ;
#11062 = CARTESIAN_POINT ( 'NONE',  ( 0.000000000000000000, 10.00000000000000000, 1.000000000000000000 ) ) ;
#11063 = VECTOR ( 'NONE', #1205, 1000.000000000000227 ) ;
#11064 = VECTOR ( 'NONE', #14243, 1000.000000000000000 ) ;
#11065 = EDGE_CURVE ( 'NONE', #12358, #14797, #8453, .T. ) ;
#11066 = VECTOR ( 'NONE', #2516, 1000.000000000000000 ) ;
#11067 = EDGE_CURVE ( 'NONE', #8973, #15262, #2532, .T. ) ;
#11068 = CIRCLE ( 'NONE', #2045, 10.00000000000000000 ) ;
#11069 = ORIENTED_EDGE ( 'NONE', *, *, #15911, .F. ) ;
#11070 = CARTESIAN_POINT ( 'NONE',  ( 9.347191417683177406, -21.22443879296941915, 1.770995438708345748 ) ) ;
#11071 = LINE ( 'NONE', #4576, #16666 ) ;
#11072 = CARTESIAN_POINT ( 'NONE',  ( -1.743623630681728542, -9.116095536440919744, 2.372946416531167557 ) ) ;
#11073 = DIRECTION ( 'NONE',  ( -1.000000000000000000, 0.000000000000000000, 0.000000000000000000 ) ) ;
#11074 = CARTESIAN_POINT ( 'NONE',  ( -10.93405858231679417, -23.20159541128345992, 4.773278322869455970 ) ) ;
#11075 = CARTESIAN_POINT ( 'NONE',  ( 12.25344141768317741, -21.94931252712233061, 1.749999999999998446 ) ) ;
#11076 = CARTESIAN_POINT ( 'NONE',  ( -18.98630159782011262, 0.000000000000000000, 1.000000000000000000 ) ) ;
#11077 = CARTESIAN_POINT ( 'NONE',  ( -10.56594141768317741, -23.20159541128344927, 2.226721677130534705 ) ) ;
#11078 = ORIENTED_EDGE ( 'NONE', *, *, #9821, .F. ) ;
#11079 = CARTESIAN_POINT ( 'NONE',  ( 5.590308582316794173, -21.32581373872472597, 1.729004561291657582 ) ) ;
#11080 = FACE_OUTER_BOUND ( 'NONE', #10860, .T. ) ;
#11081 = CARTESIAN_POINT ( 'NONE',  ( -12.67103257592000176, -18.67535491604046172, 6.269892079155907183 ) ) ;
#11082 = ORIENTED_EDGE ( 'NONE', *, *, #11845, .T. ) ;
#11083 = CARTESIAN_POINT ( 'NONE',  ( 8.215308582316792396, -23.77099543870833998, 2.825813738724734847 ) ) ;
#11084 = DIRECTION ( 'NONE',  ( 1.000000000000000000, 3.469446951953611033E-15, -0.000000000000000000 ) ) ;
#11085 = ORIENTED_EDGE ( 'NONE', *, *, #15464, .F. ) ;
#11086 = CARTESIAN_POINT ( 'NONE',  ( -0.1250000000000035805, 0.000000000000000000, 1.000000000000000000 ) ) ;
#11087 = FILL_AREA_STYLE ('',( #7538 ) ) ;
#11088 = ORIENTED_EDGE ( 'NONE', *, *, #12646, .F. ) ;
#11089 = EDGE_CURVE ( 'NONE', #607, #19969, #8343, .T. ) ;
#11090 = LINE ( 'NONE', #14206, #17144 ) ;
#11091 = EDGE_CURVE ( 'NONE', #13894, #6206, #11373, .T. ) ;
#11092 = ORIENTED_EDGE ( 'NONE', *, *, #18241, .F. ) ;
#11093 = CARTESIAN_POINT ( 'NONE',  ( -8.121558582316792396, -23.74999999999999645, 3.550687472877651629 ) ) ;
#11094 = VECTOR ( 'NONE', #19573, 1000.000000000000000 ) ;
#11095 = CARTESIAN_POINT ( 'NONE',  ( 12.62499999999998224, -20.24999999999998934, 4.291666666666698937 ) ) ;
#11096 = LINE ( 'NONE', #15889, #10157 ) ;
#11097 = CARTESIAN_POINT ( 'NONE',  ( 1.665360951492234287, -9.864914341757378580, 1.622643062139706993 ) ) ;
#11098 = CARTESIAN_POINT ( 'NONE',  ( 6.183390479346035917, 0.000000000000000000, 1.000000000000000000 ) ) ;
#11099 = CARTESIAN_POINT ( 'NONE',  ( -13.84501465882535598, 4.235740270674679842, 5.020612255068622076 ) ) ;
#11100 = CARTESIAN_POINT ( 'NONE',  ( 13.18405858231679595, -20.26807450282662160, 1.696391591240633101 ) ) ;
#11101 = CARTESIAN_POINT ( 'NONE',  ( -12.66383876651304874, -19.03864229108970463, 6.262079579155994224 ) ) ;
#11102 = EDGE_CURVE ( 'NONE', #9583, #1458, #6779, .T. ) ;
#11103 = DIRECTION ( 'NONE',  ( -0.000000000000000000, -0.000000000000000000, -1.000000000000000000 ) ) ;
#11104 = PLANE ( 'NONE',  #16092 ) ;
#11105 = VECTOR ( 'NONE', #13337, 1000.000000000000000 ) ;
#11106 = CARTESIAN_POINT ( 'NONE',  ( 8.315941417683177406, -21.32873467460645145, 4.242948236979555254 ) ) ;
#11107 = CARTESIAN_POINT ( 'NONE',  ( -5.121558582316794173, -23.74999999999999645, 3.550687472877651629 ) ) ;
#11108 = ORIENTED_EDGE ( 'NONE', *, *, #4167, .F. ) ;
#11109 = CARTESIAN_POINT ( 'NONE',  ( 13.83710853266996388, 3.836480899831821834, 5.239411421715695738 ) ) ;
#11110 = PLANE ( 'NONE',  #16684 ) ;
#11111 = ORIENTED_EDGE ( 'NONE', *, *, #17973, .F. ) ;
#11112 = UNCERTAINTY_MEASURE_WITH_UNIT (LENGTH_MEASURE( 1.000000000000000082E-05 ), #4790, 'distance_accuracy_value', 'NONE');
#11113 = VERTEX_POINT ( 'NONE', #5201 ) ;
#11114 = DIRECTION ( 'NONE',  ( 0.000000000000000000, 0.000000000000000000, -1.000000000000000000 ) ) ;
#11115 = CARTESIAN_POINT ( 'NONE',  ( 0.000000000000000000, 10.00000000000000000, 1.000000000000000000 ) ) ;
#11116 = CARTESIAN_POINT ( 'NONE',  ( -3.564229130755586006, -10.39902496812945465, 2.145043306434553987 ) ) ;
#11117 = FACE_OUTER_BOUND ( 'NONE', #2252, .T. ) ;
#11118 = VECTOR ( 'NONE', #2000, 1000.000000000000000 ) ;
#11119 = LINE ( 'NONE', #7971, #10735 ) ;
#11120 = CARTESIAN_POINT ( 'NONE',  ( -13.00900269284621302, -0.8578640112522492034, 5.903024842915844062 ) ) ;
#11121 = CARTESIAN_POINT ( 'NONE',  ( 12.15280858231679595, -21.22443879296942626, 5.229004561291660025 ) ) ;
#11122 = DIRECTION ( 'NONE',  ( 0.000000000000000000, -0.000000000000000000, 1.000000000000000000 ) ) ;
#11123 = CARTESIAN_POINT ( 'NONE',  ( 13.15384296923648400, 5.706569946443514674, 5.461568745250741763 ) ) ;
#11124 = CARTESIAN_POINT ( 'NONE',  ( 0.000000000000000000, -9.864917468222230923, 1.622643865078341241 ) ) ;
#11125 = VERTEX_POINT ( 'NONE', #11579 ) ;
#11126 = CARTESIAN_POINT ( 'NONE',  ( -13.87470602645761986, 4.985154336109792972, 3.666666666666500873 ) ) ;
#11127 = CARTESIAN_POINT ( 'NONE',  ( -10.38119784648305632, -14.00000000000000000, 1.000000000000000000 ) ) ;
#11128 = EDGE_CURVE ( 'NONE', #8745, #10713, #11268, .T. ) ;
#11129 = CARTESIAN_POINT ( 'NONE',  ( 12.15969141768317741, -22.67418626127524917, 1.729004561291651809 ) ) ;
#11130 = CARTESIAN_POINT ( 'NONE',  ( -3.944195004867014909, -21.80034658733847053, 4.481176709221804444 ) ) ;
#11131 = ORIENTED_EDGE ( 'NONE', *, *, #6418, .F. ) ;
#11132 = CARTESIAN_POINT ( 'NONE',  ( 13.87470602645761986, 4.985154336109792972, 4.166666666666765551 ) ) ;
#11133 = CARTESIAN_POINT ( 'NONE',  ( 12.62500000000001954, -20.24999999999450040, 3.833333333368183382 ) ) ;
#11134 = DIRECTION ( 'NONE',  ( 0.000000000000000000, 0.000000000000000000, 1.000000000000000000 ) ) ;
#11135 = VERTEX_POINT ( 'NONE', #16390 ) ;
#11136 = VECTOR ( 'NONE', #19895, 1000.000000000000000 ) ;
#11137 = ORIENTED_EDGE ( 'NONE', *, *, #3127, .T. ) ;
#11138 = CARTESIAN_POINT ( 'NONE',  ( 0.000000000000000000, 9.000000000000001776, 0.000000000000000000 ) ) ;
#11139 = DIRECTION ( 'NONE',  ( 0.000000000000000000, 1.000000000000000000, -0.000000000000000000 ) ) ;
#11140 = FACE_OUTER_BOUND ( 'NONE', #6433, .T. ) ;
#11141 = CARTESIAN_POINT ( 'NONE',  ( -13.12500000000000000, 5.004982103124741677, 3.999999999999983569 ) ) ;
#11142 = VECTOR ( 'NONE', #5432, 1000.000000000000000 ) ;
#11143 = PLANE ( 'NONE',  #20362 ) ;
#11144 = CARTESIAN_POINT ( 'NONE',  ( 2.747777887823422471, -9.906471667804277459, 1.825930796414880763 ) ) ;
#11145 = DIRECTION ( 'NONE',  ( 0.000000000000000000, 0.000000000000000000, 1.000000000000000000 ) ) ;
#11146 = CARTESIAN_POINT ( 'NONE',  ( 0.000000000000000000, 11.64110105645932691, 10.00000000000000000 ) ) ;
#11147 = CARTESIAN_POINT ( 'NONE',  ( 0.000000000000000000, 10.00000000000000000, 1.000000000000000000 ) ) ;
#11148 = DIRECTION ( 'NONE',  ( -0.000000000000000000, -0.000000000000000000, -1.000000000000000000 ) ) ;
#11149 = CARTESIAN_POINT ( 'NONE',  ( -12.62155858231679417, -23.74999999999999645, 3.550687472877651629 ) ) ;
#11150 = CARTESIAN_POINT ( 'NONE',  ( -2.109407804498405703, -9.207748739546751438, 2.396484790045401603 ) ) ;
#11151 = CARTESIAN_POINT ( 'NONE',  ( 7.940941417683175629, -21.25705176302044208, 2.828734674606458555 ) ) ;
#11152 = CARTESIAN_POINT ( 'NONE',  ( -13.12529380813666435, 5.014837310896125722, 5.033295791462342628 ) ) ;
#11153 = CARTESIAN_POINT ( 'NONE',  ( -7.277808582316795061, -21.02099543870833998, 3.035098964749253003 ) ) ;
#11154 = EDGE_CURVE ( 'NONE', #6649, #19533, #19642, .T. ) ;
#11155 = CARTESIAN_POINT ( 'NONE',  ( -10.94094141768317741, -20.72672167713052715, 2.298404588716546293 ) ) ;
#11156 = ORIENTED_EDGE ( 'NONE', *, *, #14680, .F. ) ;
#11157 = CARTESIAN_POINT ( 'NONE',  ( 13.37499999999998401, -19.49999999999998934, 3.146526952850934755 ) ) ;
#11158 = FILL_AREA_STYLE_COLOUR ( '', #8027 ) ;
#11159 = ORIENTED_EDGE ( 'NONE', *, *, #9585, .T. ) ;
#11160 = ORIENTED_EDGE ( 'NONE', *, *, #12931, .T. ) ;
#11161 = CARTESIAN_POINT ( 'NONE',  ( -9.999999999999998224, -30.00000000000000355, 1.000000000000000000 ) ) ;
#11162 = ORIENTED_EDGE ( 'NONE', *, *, #8154, .F. ) ;
#11163 = FACE_OUTER_BOUND ( 'NONE', #7630, .T. ) ;
#11164 = ADVANCED_FACE ( 'NONE', ( #1760 ), #3322, .T. ) ;
#11165 = EDGE_CURVE ( 'NONE', #6152, #3941, #7191, .T. ) ;
#11166 = ORIENTED_EDGE ( 'NONE', *, *, #3876, .F. ) ;
#11167 = DIRECTION ( 'NONE',  ( 1.000000000000000000, 0.000000000000000000, 0.000000000000000000 ) ) ;
#11168 = PLANE ( 'NONE',  #13636 ) ;
#11169 = CARTESIAN_POINT ( 'NONE',  ( -1.772926875221950249, -9.883376166076789815, 2.377384427436886494 ) ) ;
#11170 = LINE ( 'NONE', #19133, #6313 ) ;
#11171 = CARTESIAN_POINT ( 'NONE',  ( -11.12155858231679417, -23.74999999999999645, 3.550687472877651629 ) ) ;
#11172 = CARTESIAN_POINT ( 'NONE',  ( 5.878441417683177406, -24.50000000000000000, 3.449312527122335048 ) ) ;
#11173 = CARTESIAN_POINT ( 'NONE',  ( -12.62844141768317741, -20.99999999999999645, 3.550687472877664952 ) ) ;
#11174 = ADVANCED_FACE ( 'NONE', ( #20169 ), #15443, .T. ) ;
#11175 = ORIENTED_EDGE ( 'NONE', *, *, #13376, .F. ) ;
#11176 = CARTESIAN_POINT ( 'NONE',  ( 7.465308582316795061, -20.22900456129164937, 4.174186261275266929 ) ) ;
#11177 = DIRECTION ( 'NONE',  ( -0.000000000000000000, -0.000000000000000000, -1.000000000000000000 ) ) ;
#11178 = CARTESIAN_POINT ( 'NONE',  ( -12.68302225826488616, -18.06987595762608478, 6.282912912489355683 ) ) ;
#11179 = ORIENTED_EDGE ( 'NONE', *, *, #12449, .T. ) ;
#11180 = CARTESIAN_POINT ( 'NONE',  ( 6.527808582316794173, -23.72900456129165647, 4.275561207030568411 ) ) ;
#11181 = DIRECTION ( 'NONE',  ( 0.000000000000000000, 1.000000000000000000, 0.000000000000000000 ) ) ;
#11182 = ORIENTED_EDGE ( 'NONE', *, *, #9408, .F. ) ;
#11183 = DIRECTION ( 'NONE',  ( 1.000000000000000000, 0.000000000000000000, 0.000000000000000000 ) ) ;
#11184 = DIRECTION ( 'NONE',  ( 1.000000000000000000, 0.000000000000000000, 0.000000000000000000 ) ) ;
#11185 = ORIENTED_EDGE ( 'NONE', *, *, #18314, .T. ) ;
#11186 = LINE ( 'NONE', #3138, #1445 ) ;
#11187 = ORIENTED_EDGE ( 'NONE', *, *, #14623, .F. ) ;
#11188 = ADVANCED_FACE ( 'NONE', ( #18275 ), #8862, .T. ) ;
#11189 = CARTESIAN_POINT ( 'NONE',  ( -6.152808582316793284, -21.22443879296942626, 5.229004561291659137 ) ) ;
#11190 = CARTESIAN_POINT ( 'NONE',  ( 12.64571531779736979, -19.20387645123237164, 5.508493592915143289 ) ) ;
#11191 = CARTESIAN_POINT ( 'NONE',  ( 6.813547257480585095, 11.64110105645932691, 0.000000000000000000 ) ) ;
#11192 = CARTESIAN_POINT ( 'NONE',  ( 2.041623931606483033, -10.12028065167953272, 1.688226231982305370 ) ) ;
#11193 = PLANE ( 'NONE',  #17023 ) ;
#11194 = CARTESIAN_POINT ( 'NONE',  ( -13.84476264919594612, 4.223013784394161974, 5.079233071712400793 ) ) ;
#11195 = CARTESIAN_POINT ( 'NONE',  ( 5.871558582316794173, -20.24999999999999289, 3.449312527122348371 ) ) ;
#11196 = CARTESIAN_POINT ( 'NONE',  ( -13.90258797164900884, 5.643192568275169130, 5.568788873356017355 ) ) ;
#11197 = EDGE_CURVE ( 'NONE', #5735, #1111, #20064, .T. ) ;
#11198 = EDGE_CURVE ( 'NONE', #4337, #8442, #2573, .T. ) ;
#11199 = FACE_OUTER_BOUND ( 'NONE', #1509, .T. ) ;
#11200 = CARTESIAN_POINT ( 'NONE',  ( -5.684058582316795949, -20.26807450282662160, 1.696391591240633101 ) ) ;
#11201 = CARTESIAN_POINT ( 'NONE',  ( 8.871558582316794173, -20.24999999999999289, 3.449312527122348371 ) ) ;
#11202 = AXIS2_PLACEMENT_3D ( 'NONE', #4295, #10790, #16943 ) ;
#11203 = VECTOR ( 'NONE', #2759, 1000.000000000000000 ) ;
#11204 = CARTESIAN_POINT ( 'NONE',  ( 13.37155858231679595, -20.99999999999999645, 3.449312527122348371 ) ) ;
#11205 = CARTESIAN_POINT ( 'NONE',  ( -9.722191417683177406, -20.27099543870833998, 4.275561207030583510 ) ) ;
#11206 = ORIENTED_EDGE ( 'NONE', *, *, #17229, .T. ) ;
#11207 = CARTESIAN_POINT ( 'NONE',  ( 13.84495141469777479, 4.232546442235974204, 5.040078719623224401 ) ) ;
#11208 = DIRECTION ( 'NONE',  ( -0.000000000000000000, 0.000000000000000000, -1.000000000000000000 ) ) ;
#11209 = ORIENTED_EDGE ( 'NONE', *, *, #7759, .T. ) ;
#11210 = ORIENTED_EDGE ( 'NONE', *, *, #11091, .T. ) ;
#11211 = CARTESIAN_POINT ( 'NONE',  ( 27.49999999999999645, -4.770489558936219510E-14, 0.000000000000000000 ) ) ;
#11212 = LINE ( 'NONE', #6717, #14712 ) ;
#11213 = EDGE_CURVE ( 'NONE', #15304, #8944, #19751, .T. ) ;
#11214 = CARTESIAN_POINT ( 'NONE',  ( 15.00000000000001421, -17.49999999999999645, 4.000000000000000000 ) ) ;
#11215 = CARTESIAN_POINT ( 'NONE',  ( -1.548630333695928618, -8.364917468222230923, 2.372643865078341019 ) ) ;
#11216 = CARTESIAN_POINT ( 'NONE',  ( -7.369520639128046113, 0.000000000000000000, 1.000000000000000000 ) ) ;
#11217 = CARTESIAN_POINT ( 'NONE',  ( -14.49999999999998579, -18.49999999999999645, 1.000000000000000000 ) ) ;
#11218 = CARTESIAN_POINT ( 'NONE',  ( -13.11145189917479392, 4.315820908324673688, 5.961432613039677086 ) ) ;
#11219 = CARTESIAN_POINT ( 'NONE',  ( 8.126396343307449754, 10.00000000000000000, 1.000000000000000000 ) ) ;
#11220 = CARTESIAN_POINT ( 'NONE',  ( -9.999999999999996447, -34.99999999999999289, 1.000000000000000000 ) ) ;
#11221 = CARTESIAN_POINT ( 'NONE',  ( 13.12405442816082868, 4.202248622120948518, 6.747400073346936367 ) ) ;
#11222 = CARTESIAN_POINT ( 'NONE',  ( -1.853238653218509890, -9.965882697426144077, 2.398573752920997837 ) ) ;
#11223 = VERTEX_POINT ( 'NONE', #8760 ) ;
#11224 = CARTESIAN_POINT ( 'NONE',  ( -13.87367531042247748, 4.933103176334663331, 5.324010972534209074 ) ) ;
#11225 = DIRECTION ( 'NONE',  ( 1.000000000000000000, 1.734723475976787570E-15, 0.000000000000000000 ) ) ;
#11226 = CARTESIAN_POINT ( 'NONE',  ( 5.409691417683178294, -21.01515356694492098, 6.020995438708349745 ) ) ;
#11227 = CARTESIAN_POINT ( 'NONE',  ( -6.815941417683177406, -21.32873467460645145, 4.242948236979555254 ) ) ;
#11228 = ORIENTED_EDGE ( 'NONE', *, *, #11944, .T. ) ;
#11229 = CARTESIAN_POINT ( 'NONE',  ( 12.62505438222622622, -20.99725369757571869, 4.613400783263607252 ) ) ;
#11230 = CARTESIAN_POINT ( 'NONE',  ( 12.62499999999998401, -19.49999999999998934, 3.666666666666654084 ) ) ;
#11231 = CARTESIAN_POINT ( 'NONE',  ( -7.500000000000000000, -19.49999999999999645, 5.000000000000000000 ) ) ;
#11232 = ORIENTED_EDGE ( 'NONE', *, *, #17929, .F. ) ;
#11233 = ORIENTED_EDGE ( 'NONE', *, *, #14713, .F. ) ;
#11234 = LINE ( 'NONE', #17725, #20484 ) ;
#11235 = EDGE_CURVE ( 'NONE', #17247, #3944, #4251, .T. ) ;
#11236 = DIRECTION ( 'NONE',  ( 8.673617379884045333E-17, -1.000000000000000000, 0.000000000000000000 ) ) ;
#11237 = CARTESIAN_POINT ( 'NONE',  ( 24.50000000000000000, 0.000000000000000000, 0.000000000000000000 ) ) ;
#11238 = CARTESIAN_POINT ( 'NONE',  ( -22.81633994409548549, 10.00000000000000000, 1.000000000000000000 ) ) ;
#11239 = CARTESIAN_POINT ( 'NONE',  ( 1.407845757905374695, -9.114917468222230923, 1.622643865078341463 ) ) ;
#11240 = CARTESIAN_POINT ( 'NONE',  ( 15.36404127825609400, 9.000000000000001776, 1.000000000000000000 ) ) ;
#11241 = FACE_OUTER_BOUND ( 'NONE', #8107, .T. ) ;
#11242 = CARTESIAN_POINT ( 'NONE',  ( -27.52582389412042474, 4.853545418763153485, 1.000000000000000000 ) ) ;
#11243 = DIRECTION ( 'NONE',  ( 0.000000000000000000, 0.1264857625231113059, -0.9919684228235025047 ) ) ;
#11244 = CARTESIAN_POINT ( 'NONE',  ( -12.15280858231679595, -21.22443879296942626, 5.229004561291659137 ) ) ;
#11245 = FACE_OUTER_BOUND ( 'NONE', #10278, .T. ) ;
#11246 = CARTESIAN_POINT ( 'NONE',  ( 9.715308582316795949, -23.02099543870833998, 3.136473910504556262 ) ) ;
#11247 = CARTESIAN_POINT ( 'NONE',  ( -12.62503976493681535, -19.49799187068907713, 4.533161381885315144 ) ) ;
#11248 = CARTESIAN_POINT ( 'NONE',  ( -13.18405858231679417, -20.79840458871652942, 2.226721677130544030 ) ) ;
#11249 = CARTESIAN_POINT ( 'NONE',  ( -11.31594141768317741, -20.79840458871654363, 4.773278322869464851 ) ) ;
#11250 = ORIENTED_EDGE ( 'NONE', *, *, #6418, .T. ) ;
#11251 = CARTESIAN_POINT ( 'NONE',  ( 13.37908441539295801, -19.29373702265862889, 4.740102594697787275 ) ) ;
#11252 = CARTESIAN_POINT ( 'NONE',  ( 0.000000000000000000, 16.00000000000000000, 1.000000000000000000 ) ) ;
#11253 = EDGE_LOOP ( 'NONE', ( #6467, #17376, #12658, #15006 ) ) ;
#11254 = VERTEX_POINT ( 'NONE', #807 ) ;
#11255 = CARTESIAN_POINT ( 'NONE',  ( 14.99999999999999645, 3.000000000000003553, 2.000000000000000000 ) ) ;
#11256 = ORIENTED_EDGE ( 'NONE', *, *, #14213, .T. ) ;
#11257 = PLANE ( 'NONE',  #5089 ) ;
#11258 = ORIENTED_EDGE ( 'NONE', *, *, #19165, .T. ) ;
#11259 = CARTESIAN_POINT ( 'NONE',  ( 10.65969141768317918, -22.67418626127524917, 1.729004561291651587 ) ) ;
#11260 = CARTESIAN_POINT ( 'NONE',  ( -1.561130159782011306, 4.999999999999999112, 1.000000000000000000 ) ) ;
#11261 = EDGE_CURVE ( 'NONE', #19679, #17944, #7089, .T. ) ;
#11262 = CARTESIAN_POINT ( 'NONE',  ( -2.623717082130370137, -10.12934627674766830, 2.633169448359191644 ) ) ;
#11263 = DIRECTION ( 'NONE',  ( 0.000000000000000000, -1.000000000000000000, 1.304178812473495102E-15 ) ) ;
#11264 = CARTESIAN_POINT ( 'NONE',  ( -13.37327929115833491, -20.24999999560066399, 3.449077790995343840 ) ) ;
#11265 = ADVANCED_FACE ( 'NONE', ( #16694 ), #12561, .T. ) ;
#11266 = EDGE_CURVE ( 'NONE', #4517, #11657, #15237, .T. ) ;
#11267 = CARTESIAN_POINT ( 'NONE',  ( 12.15969141768317741, -22.67418626127524917, 1.729004561291651809 ) ) ;
#11268 = LINE ( 'NONE', #2164, #19587 ) ;
#11269 = CARTESIAN_POINT ( 'NONE',  ( -4.565941417683176518, -23.20159541128344927, 2.226721677130534705 ) ) ;
#11270 = ORIENTED_EDGE ( 'NONE', *, *, #11571, .F. ) ;
#11271 = CARTESIAN_POINT ( 'NONE',  ( 12.05905858231679595, -20.19639159124062999, 5.231925497173373074 ) ) ;
#11272 = DIRECTION ( 'NONE',  ( -1.000000000000000000, 0.000000000000000000, 0.000000000000000000 ) ) ;
#11273 = CARTESIAN_POINT ( 'NONE',  ( -12.62499999999998401, -20.99999999999998934, 2.439580858552613751 ) ) ;
#11274 = ORIENTED_EDGE ( 'NONE', *, *, #5705, .T. ) ;
#11275 = VECTOR ( 'NONE', #3135, 1000.000000000000000 ) ;
#11276 = CARTESIAN_POINT ( 'NONE',  ( 5.215308582316793284, -23.77099543870833998, 2.825813738724734847 ) ) ;
#11277 = CARTESIAN_POINT ( 'NONE',  ( -2.499999999999998224, -24.49999999999999289, 1.000000000000000000 ) ) ;
#11278 = ORIENTED_EDGE ( 'NONE', *, *, #18376, .F. ) ;
#11279 = DIRECTION ( 'NONE',  ( 0.000000000000000000, 0.000000000000000000, 1.000000000000000000 ) ) ;
#11280 = DIRECTION ( 'NONE',  ( 1.000000000000000000, 0.000000000000000000, 0.000000000000000000 ) ) ;
#11281 = EDGE_LOOP ( 'NONE', ( #430, #8751, #11893, #12581 ) ) ;
#11282 = DIRECTION ( 'NONE',  ( 0.000000000000000000, 0.000000000000000000, -1.000000000000000000 ) ) ;
#11283 = ORIENTED_EDGE ( 'NONE', *, *, #5387, .T. ) ;
#11284 = CARTESIAN_POINT ( 'NONE',  ( -5.496558582316794173, -22.05068747287764452, 1.749999999999998446 ) ) ;
#11285 = CARTESIAN_POINT ( 'NONE',  ( 0.000000000000000000, 9.000000000000001776, 1.000000000000000000 ) ) ;
#11286 = ADVANCED_FACE ( 'NONE', ( #13659 ), #6143, .T. ) ;
#11287 = CARTESIAN_POINT ( 'NONE',  ( 0.000000000000000000, 9.000000000000001776, 0.000000000000000000 ) ) ;
#11288 = CARTESIAN_POINT ( 'NONE',  ( 1.776440835594205847, -9.874406767442327038, 1.625080906685880233 ) ) ;
#11289 = CARTESIAN_POINT ( 'NONE',  ( 12.79798428357658047, -11.51429367935891790, 5.673858176248284479 ) ) ;
#11290 = LINE ( 'NONE', #14316, #16688 ) ;
#11291 = CARTESIAN_POINT ( 'NONE',  ( -13.83710853266996388, 3.836480899831821834, 5.239411421715695738 ) ) ;
#11292 = CARTESIAN_POINT ( 'NONE',  ( 7.559058582316794173, -20.72672167713054137, 4.701595411283463477 ) ) ;
#11293 = CARTESIAN_POINT ( 'NONE',  ( -13.90439735423812273, 5.734566389025032684, 4.833333333333343695 ) ) ;
#11294 = CARTESIAN_POINT ( 'NONE',  ( 15.00000000000000355, -5.999999999999996447, 1.000000000000000000 ) ) ;
#11295 = CARTESIAN_POINT ( 'NONE',  ( -8.777808582316797725, -19.52099543870833642, 2.413778621189609286 ) ) ;
#11296 = CARTESIAN_POINT ( 'NONE',  ( 6.340308582316793284, -22.67418626127525982, 5.270995438708342640 ) ) ;
#11297 = EDGE_CURVE ( 'NONE', #7639, #4697, #6348, .T. ) ;
#11298 = CARTESIAN_POINT ( 'NONE',  ( 8.878441417683177406, -22.99999999999999645, 3.449312527122335048 ) ) ;
#11299 = CARTESIAN_POINT ( 'NONE',  ( -8.503441417683177406, -22.05068747287765873, 5.250000000000000888 ) ) ;
#11300 = VECTOR ( 'NONE', #10765, 1000.000000000000000 ) ;
#11301 = ORIENTED_EDGE ( 'NONE', *, *, #13881, .T. ) ;
#11302 = EDGE_LOOP ( 'NONE', ( #7604, #18043, #6432, #4085 ) ) ;
#11303 = CARTESIAN_POINT ( 'NONE',  ( 13.37499999999998224, -20.24999999999998934, 4.291666666666698937 ) ) ;
#11304 = CYLINDRICAL_SURFACE ( 'NONE', #19471, 10.00000000000000000 ) ;
#11305 = CARTESIAN_POINT ( 'NONE',  ( -20.75349085826862350, 16.00000000000000000, 1.000000000000000000 ) ) ;
#11306 = VECTOR ( 'NONE', #6473, 1000.000000000000000 ) ;
#11307 = ORIENTED_EDGE ( 'NONE', *, *, #13064, .T. ) ;
#11308 = ORIENTED_EDGE ( 'NONE', *, *, #12509, .T. ) ;
#11309 = PLANE ( 'NONE',  #13450 ) ;
#11310 = LINE ( 'NONE', #5237, #16048 ) ;
#11311 = PLANE ( 'NONE',  #6927 ) ;
#11312 = EDGE_CURVE ( 'NONE', #8687, #17482, #1635, .T. ) ;
#11313 = ADVANCED_FACE ( 'NONE', ( #20378 ), #2899, .T. ) ;
#11314 = CARTESIAN_POINT ( 'NONE',  ( -1.619022621591186928, -8.364917468222230923, 2.372643865078341019 ) ) ;
#11315 = CARTESIAN_POINT ( 'NONE',  ( 1.655860418491166941, -9.114909740826840689, 2.372641880528837621 ) ) ;
#11316 = VECTOR ( 'NONE', #15301, 1000.000000000000000 ) ;
#11317 = CARTESIAN_POINT ( 'NONE',  ( -15.00000000000000000, 3.000000000000000000, 2.000000000000000000 ) ) ;
#11318 = CARTESIAN_POINT ( 'NONE',  ( -12.74043380832193684, -14.42059267975384529, 5.611358176248560703 ) ) ;
#11319 = CARTESIAN_POINT ( 'NONE',  ( 12.71530858231679417, -23.77099543870833998, 2.825813738724734847 ) ) ;
#11320 = DIRECTION ( 'NONE',  ( 0.000000000000000000, 0.000000000000000000, -1.000000000000000000 ) ) ;
#11321 = CARTESIAN_POINT ( 'NONE',  ( 12.62499999999998224, -20.24999999999998934, 4.166666666666636765 ) ) ;
#11322 = CARTESIAN_POINT ( 'NONE',  ( -1.337453470010121714, -9.864917468222230923, 1.622643865078341907 ) ) ;
#11323 = EDGE_LOOP ( 'NONE', ( #9893, #15110, #15951, #3491, #6070 ) ) ;
#11324 = CARTESIAN_POINT ( 'NONE',  ( -13.87470602645761986, 4.985154336109792972, 4.583333333333296622 ) ) ;
#11325 = DIRECTION ( 'NONE',  ( 1.000000000000000000, 0.000000000000000000, -0.000000000000000000 ) ) ;
#11326 = CARTESIAN_POINT ( 'NONE',  ( 7.097191417683176518, -23.08622137881040359, 5.979004561291654696 ) ) ;
#11327 = CARTESIAN_POINT ( 'NONE',  ( -10.37155858231679595, -20.99999999999999645, 3.449312527122348371 ) ) ;
#11328 = VERTEX_POINT ( 'NONE', #12412 ) ;
#11329 = CARTESIAN_POINT ( 'NONE',  ( 13.86796007304617717, 3.894483688830428836, 6.740724019197413597 ) ) ;
#11330 = CARTESIAN_POINT ( 'NONE',  ( 13.12529397354238192, 5.014845663890295846, 4.916666666666650087 ) ) ;
#11331 = CIRCLE ( 'NONE', #1644, 0.3749999999999997224 ) ;
#11332 = VECTOR ( 'NONE', #3730, 1000.000000000000000 ) ;
#11333 = DIRECTION ( 'NONE',  ( -0.000000000000000000, 0.000000000000000000, -1.000000000000000000 ) ) ;
#11334 = VERTEX_POINT ( 'NONE', #14178 ) ;
#11335 = VECTOR ( 'NONE', #8659, 1000.000000000000114 ) ;
#11336 = ORIENTED_EDGE ( 'NONE', *, *, #1988, .F. ) ;
#11337 = DIRECTION ( 'NONE',  ( -0.000000000000000000, -0.000000000000000000, -1.000000000000000000 ) ) ;
#11338 = LINE ( 'NONE', #17726, #8570 ) ;
#11339 = ORIENTED_EDGE ( 'NONE', *, *, #18283, .T. ) ;
#11340 = CARTESIAN_POINT ( 'NONE',  ( 7.499999999999999112, -25.49999999999999645, 4.000000000000000000 ) ) ;
#11341 = CARTESIAN_POINT ( 'NONE',  ( 1.865667289525601680, -9.999006358835732300, 2.407080570882605297 ) ) ;
#11342 = CARTESIAN_POINT ( 'NONE',  ( -14.99999999999998224, -17.49999999999999645, 4.000000000000000000 ) ) ;
#11343 = VECTOR ( 'NONE', #896, 1000.000000000000000 ) ;
#11344 = LINE ( 'NONE', #14482, #3756 ) ;
#11345 = CARTESIAN_POINT ( 'NONE',  ( 13.12529397354238192, 5.014845663890297622, 3.999999999999981792 ) ) ;
#11346 = AXIS2_PLACEMENT_3D ( 'NONE', #16, #18755, #9224 ) ;
#11347 = DIRECTION ( 'NONE',  ( -0.000000000000000000, -0.000000000000000000, -1.000000000000000000 ) ) ;
#11348 = CARTESIAN_POINT ( 'NONE',  ( -3.277163086644854229, -14.76879761173520578, 3.824673233536266537 ) ) ;
#11349 = PRODUCT_DEFINITION_SHAPE ( 'NONE', 'NONE',  #20724 ) ;
#11350 = CARTESIAN_POINT ( 'NONE',  ( -12.62515856830665584, -19.49199230051052822, 4.565864671500353467 ) ) ;
#11351 = CARTESIAN_POINT ( 'NONE',  ( -5.684058582316795949, -21.32873467460644079, 2.757051763020455404 ) ) ;
#11352 = EDGE_CURVE ( 'NONE', #17295, #1310, #18910, .T. ) ;
#11353 = VECTOR ( 'NONE', #14483, 1000.000000000000000 ) ;
#11354 = CARTESIAN_POINT ( 'NONE',  ( -7.753441417683176518, -21.94931252712233061, 1.749999999999998446 ) ) ;
#11355 = ORIENTED_EDGE ( 'NONE', *, *, #13999, .F. ) ;
#11356 = CARTESIAN_POINT ( 'NONE',  ( 13.82811627091129836, 3.382371681020614584, 5.229645796715683304 ) ) ;
#11357 = DIRECTION ( 'NONE',  ( 0.000000000000000000, 1.000000000000000000, -0.000000000000000000 ) ) ;
#11358 = ORIENTED_EDGE ( 'NONE', *, *, #15091, .T. ) ;
#11359 = ORIENTED_EDGE ( 'NONE', *, *, #4045, .T. ) ;
#11360 = CARTESIAN_POINT ( 'NONE',  ( 0.000000000000000000, 4.999999999999999112, 1.000000000000000000 ) ) ;
#11361 = ORIENTED_EDGE ( 'NONE', *, *, #11546, .F. ) ;
#11362 = DIRECTION ( 'NONE',  ( 0.000000000000000000, 0.000000000000000000, 1.000000000000000000 ) ) ;
#11363 =( GEOMETRIC_REPRESENTATION_CONTEXT ( 3 ) GLOBAL_UNCERTAINTY_ASSIGNED_CONTEXT ( ( #12155 ) ) GLOBAL_UNIT_ASSIGNED_CONTEXT ( ( #6380, #12538, #20517 ) ) REPRESENTATION_CONTEXT ( 'NONE', 'WORKASPACE' ) );
#11364 = ORIENTED_EDGE ( 'NONE', *, *, #4226, .F. ) ;
#11365 = CARTESIAN_POINT ( 'NONE',  ( 11.31594141768317741, -20.79840458871654363, 4.773278322869464851 ) ) ;
#11366 = LINE ( 'NONE', #8334, #6650 ) ;
#11367 = VECTOR ( 'NONE', #2105, 1000.000000000000000 ) ;
#11368 = CARTESIAN_POINT ( 'NONE',  ( -1.732184490400474175, -9.869581059509965115, 2.373841568485653308 ) ) ;
#11369 = CARTESIAN_POINT ( 'NONE',  ( 2.367358971471363649, -9.400572650371021410, 2.446005822389718087 ) ) ;
#11370 = DIRECTION ( 'NONE',  ( 1.000000000000000000, 0.000000000000000000, 0.000000000000000000 ) ) ;
#11371 = CARTESIAN_POINT ( 'NONE',  ( 15.36404127825609400, 0.000000000000000000, 0.000000000000000000 ) ) ;
#11372 = CARTESIAN_POINT ( 'NONE',  ( 9.628441417683177406, -20.24999999999999289, 3.550687472877664952 ) ) ;
#11373 = LINE ( 'NONE', #16090, #4545 ) ;
#11374 = CARTESIAN_POINT ( 'NONE',  ( -4.940941417683177406, -20.72672167713052715, 2.298404588716546293 ) ) ;
#11375 = ORIENTED_EDGE ( 'NONE', *, *, #11640, .F. ) ;
#11376 = CARTESIAN_POINT ( 'NONE',  ( 9.059058582316795949, -20.19639159124062999, 5.231925497173373074 ) ) ;
#11377 = CARTESIAN_POINT ( 'NONE',  ( 13.11145189917479392, 4.315820908324673688, 5.961432613039677086 ) ) ;
#11378 = CARTESIAN_POINT ( 'NONE',  ( -13.12860732321105139, 4.432169822159808703, 6.709107302035562270 ) ) ;
#11379 = ORIENTED_EDGE ( 'NONE', *, *, #732, .F. ) ;
#11380 = VECTOR ( 'NONE', #3381, 1000.000000000000000 ) ;
#11381 = EDGE_CURVE ( 'NONE', #11591, #6263, #14310, .T. ) ;
#11382 = CARTESIAN_POINT ( 'NONE',  ( -3.500698171653725765, 11.64110105645932691, 10.00000000000000000 ) ) ;
#11383 = CARTESIAN_POINT ( 'NONE',  ( -17.11324865405191176, -11.00000000000000000, 2.000000000000000000 ) ) ;
#11384 = VECTOR ( 'NONE', #19589, 1000.000000000000000 ) ;
#11385 = ORIENTED_EDGE ( 'NONE', *, *, #330, .F. ) ;
#11386 = VECTOR ( 'NONE', #173, 1000.000000000000000 ) ;
#11387 = DIRECTION ( 'NONE',  ( 1.000000000000000000, 0.000000000000000000, 0.000000000000000000 ) ) ;
#11388 = AXIS2_PLACEMENT_3D ( 'NONE', #8727, #13119, #9877 ) ;
#11389 = ORIENTED_EDGE ( 'NONE', *, *, #10991, .T. ) ;
#11390 = CARTESIAN_POINT ( 'NONE',  ( 13.37499999932878048, -20.20702557250647047, 3.448843586020831964 ) ) ;
#11391 = EDGE_CURVE ( 'NONE', #1866, #20635, #20488, .T. ) ;
#11392 = ORIENTED_EDGE ( 'NONE', *, *, #6706, .F. ) ;
#11393 = CARTESIAN_POINT ( 'NONE',  ( -13.18405858231679595, -20.26807450282662160, 1.696391591240633101 ) ) ;
#11394 = CARTESIAN_POINT ( 'NONE',  ( -7.499999999999999112, -18.49999999999999645, 4.000000000000000000 ) ) ;
#11395 = CARTESIAN_POINT ( 'NONE',  ( 14.50000000000001243, -18.49999999999999645, 1.000000000000000000 ) ) ;
#11396 = AXIS2_PLACEMENT_3D ( 'NONE', #2116, #17908, #19592 ) ;
#11397 = CARTESIAN_POINT ( 'NONE',  ( 12.64691428603184242, -19.14332855539073464, 5.509795676248469221 ) ) ;
#11398 = DIRECTION ( 'NONE',  ( 1.000000000000000000, -0.000000000000000000, 0.000000000000000000 ) ) ;
#11399 = CARTESIAN_POINT ( 'NONE',  ( -13.84501469867711698, 4.235742283194553259, 4.333333333333380999 ) ) ;
#11400 = CARTESIAN_POINT ( 'NONE',  ( 12.15280858231679950, -20.91377862118960351, 5.979004561291660913 ) ) ;
#11401 = CARTESIAN_POINT ( 'NONE',  ( -12.73577686058281344, -15.40576854059989920, 6.340204579155907183 ) ) ;
#11402 = CARTESIAN_POINT ( 'NONE',  ( -11.97219141768317918, -24.47900456129165292, 2.413778621189595963 ) ) ;
#11403 = PLANE ( 'NONE',  #9058 ) ;
#11404 = DIRECTION ( 'NONE',  ( -1.000000000000000000, 0.000000000000000000, 0.000000000000000000 ) ) ;
#11405 = EDGE_CURVE ( 'NONE', #17531, #19533, #14387, .T. ) ;
#11406 = CARTESIAN_POINT ( 'NONE',  ( 8.871558582316795949, -20.99999999999999645, 3.449312527122348371 ) ) ;
#11407 = CARTESIAN_POINT ( 'NONE',  ( -7.003441417683177406, -22.05068747287765873, 5.250000000000000888 ) ) ;
#11408 = ORIENTED_EDGE ( 'NONE', *, *, #3787, .T. ) ;
#11409 = EDGE_LOOP ( 'NONE', ( #7461, #15498, #3481, #11564 ) ) ;
#11410 = CARTESIAN_POINT ( 'NONE',  ( 13.76337198624852398, 0.1127853055781036368, 5.159333296715827188 ) ) ;
#11411 = DIRECTION ( 'NONE',  ( 1.000000000000000000, -0.000000000000000000, 0.000000000000000000 ) ) ;
#11412 = LINE ( 'NONE', #12872, #9693 ) ;
#11413 = ORIENTED_EDGE ( 'NONE', *, *, #12162, .T. ) ;
#11414 = VECTOR ( 'NONE', #2820, 1000.000000000000000 ) ;
#11415 = ORIENTED_EDGE ( 'NONE', *, *, #17759, .T. ) ;
#11416 = CARTESIAN_POINT ( 'NONE',  ( -3.944195004867014909, -21.61378581760806128, 5.207602947182413011 ) ) ;
#11417 = EDGE_CURVE ( 'NONE', #18461, #20067, #3109, .T. ) ;
#11418 = EDGE_CURVE ( 'NONE', #10336, #16327, #9379, .T. ) ;
#11419 = DIRECTION ( 'NONE',  ( 0.000000000000000000, 0.000000000000000000, -1.000000000000000000 ) ) ;
#11420 = CARTESIAN_POINT ( 'NONE',  ( -13.12526104302547836, 5.013182672784613381, 5.066812735559260261 ) ) ;
#11421 = CARTESIAN_POINT ( 'NONE',  ( 0.000000000000000000, 16.00000000000000000, 1.000000000000000000 ) ) ;
#11422 = CARTESIAN_POINT ( 'NONE',  ( -3.521144778809589315, -10.09312707791070096, 2.066482617302010105 ) ) ;
#11423 = LINE ( 'NONE', #7446, #10062 ) ;
#11424 = CARTESIAN_POINT ( 'NONE',  ( -13.10252221513633941, 3.864871864382954048, 6.004587342915129966 ) ) ;
#11425 = SURFACE_STYLE_USAGE ( .BOTH. , #5048 ) ;
#11426 = CARTESIAN_POINT ( 'NONE',  ( 12.00000000000000178, -26.50000000000000355, 4.000000000000000000 ) ) ;
#11427 = CARTESIAN_POINT ( 'NONE',  ( 13.02818618459764188, 0.1109023222084986743, 5.923858176248589125 ) ) ;
#11428 = VECTOR ( 'NONE', #16183, 1000.000000000000000 ) ;
#11429 = PLANE ( 'NONE',  #2679 ) ;
#11430 = ORIENTED_EDGE ( 'NONE', *, *, #16997, .T. ) ;
#11431 = CARTESIAN_POINT ( 'NONE',  ( -13.54769662923970763, -11.52882022337116119, 5.659013032956382361 ) ) ;
#11432 = DIRECTION ( 'NONE',  ( 0.000000000000000000, 1.000000000000000000, -0.000000000000000000 ) ) ;
#11433 = EDGE_CURVE ( 'NONE', #19789, #4981, #9175, .T. ) ;
#11434 = CARTESIAN_POINT ( 'NONE',  ( 8.503441417683177406, -22.05068747287766229, 6.000000000000001776 ) ) ;
#11435 = CARTESIAN_POINT ( 'NONE',  ( -6.902808582316795949, -22.46490103525074034, 2.520995438708341307 ) ) ;
#11436 = VERTEX_POINT ( 'NONE', #10953 ) ;
#11437 = CARTESIAN_POINT ( 'NONE',  ( 13.84997554952896515, 2.986265251207539606, 6.721192769197450012 ) ) ;
#11438 = CARTESIAN_POINT ( 'NONE',  ( 13.12270769621861355, 4.884238659038159902, 5.513847264053151065 ) ) ;
#11439 = LINE ( 'NONE', #2023, #15014 ) ;
#11440 = VECTOR ( 'NONE', #16425, 1000.000000000000000 ) ;
#11441 = EDGE_LOOP ( 'NONE', ( #2273, #16789, #13742, #8277 ) ) ;
#11442 = ORIENTED_EDGE ( 'NONE', *, *, #7490, .F. ) ;
#11443 = CARTESIAN_POINT ( 'NONE',  ( -9.805650798910056309, 0.000000000000000000, 1.000000000000000000 ) ) ;
#11444 = VECTOR ( 'NONE', #4423, 1000.000000000000000 ) ;
#11445 = LINE ( 'NONE', #6437, #20261 ) ;
#11446 = DIRECTION ( 'NONE',  ( 0.000000000000000000, -0.000000000000000000, -1.000000000000000000 ) ) ;
#11447 = ADVANCED_FACE ( 'NONE', ( #3004 ), #4667, .T. ) ;
#11448 = CARTESIAN_POINT ( 'NONE',  ( 13.87500000000000000, 5.000000000000049738, 4.000000000000001776 ) ) ;
#11449 = CARTESIAN_POINT ( 'NONE',  ( 1.866357130655357688, -10.00562759449716133, 2.408781036472938730 ) ) ;
#11450 = DIRECTION ( 'NONE',  ( -1.000000000000000000, 0.000000000000000000, 0.000000000000000000 ) ) ;
#11451 = CARTESIAN_POINT ( 'NONE',  ( -5.381197846483055436, -14.00000000000000000, 1.000000000000000000 ) ) ;
#11452 = PLANE ( 'NONE',  #10702 ) ;
#11453 = CARTESIAN_POINT ( 'NONE',  ( -14.49999999999998579, -25.49999999999999645, 4.000000000000000000 ) ) ;
#11454 = DIRECTION ( 'NONE',  ( 1.000000000000000000, 0.000000000000000000, 0.000000000000000000 ) ) ;
#11455 = CARTESIAN_POINT ( 'NONE',  ( -1.619022621591187150, -9.114917468222230923, 2.372643865078341019 ) ) ;
#11456 = VERTEX_POINT ( 'NONE', #8017 ) ;
#11457 = CARTESIAN_POINT ( 'NONE',  ( -13.09106898171683930, 4.036483576700608644, 5.256123545019964816 ) ) ;
#11458 = CARTESIAN_POINT ( 'NONE',  ( -5.590308582316795949, -21.63647391050454871, 2.479004561291657804 ) ) ;
#11459 = AXIS2_PLACEMENT_3D ( 'NONE', #13060, #13161, #19352 ) ;
#11460 = EDGE_CURVE ( 'NONE', #8046, #12514, #7359, .T. ) ;
#11461 = CARTESIAN_POINT ( 'NONE',  ( -9.628441417683177406, -20.24999999999999289, 3.550687472877664952 ) ) ;
#11462 = VERTEX_POINT ( 'NONE', #15550 ) ;
#11463 = ADVANCED_FACE ( 'NONE', ( #1533 ), #7913, .F. ) ;
#11464 = CARTESIAN_POINT ( 'NONE',  ( 13.84501469867711698, 4.235742283194553259, 4.916666666666649199 ) ) ;
#11465 = LINE ( 'NONE', #8436, #6048 ) ;
#11466 = VERTEX_POINT ( 'NONE', #14276 ) ;
#11467 = ORIENTED_EDGE ( 'NONE', *, *, #1937, .F. ) ;
#11468 = PLANE ( 'NONE',  #16743 ) ;
#11469 = VERTEX_POINT ( 'NONE', #19120 ) ;
#11470 = CARTESIAN_POINT ( 'NONE',  ( 9.555650798910054533, 0.000000000000000000, 1.000000000000000000 ) ) ;
#11471 = VECTOR ( 'NONE', #1259, 1000.000000000000000 ) ;
#11472 = MANIFOLD_SOLID_BREP ( 'Mirror1', #14638 ) ;
#11473 = ORIENTED_EDGE ( 'NONE', *, *, #7013, .T. ) ;
#11474 = CARTESIAN_POINT ( 'NONE',  ( 4.003441417683176518, -22.05068747287765873, 5.250000000000000888 ) ) ;
#11475 = EDGE_CURVE ( 'NONE', #16571, #19021, #4773, .T. ) ;
#11476 = DIRECTION ( 'NONE',  ( -1.000000000000000000, 0.000000000000000000, 0.000000000000000000 ) ) ;
#11477 = CARTESIAN_POINT ( 'NONE',  ( -0.2815691515810352374, -9.864917468222230923, 2.372643865078523540 ) ) ;
#11478 = CARTESIAN_POINT ( 'NONE',  ( 1.957016269584227031, -9.152392576945766578, 2.382268221639079364 ) ) ;
#11479 = CARTESIAN_POINT ( 'NONE',  ( -9.246558582316794173, -21.94931252712234482, 5.250000000000000888 ) ) ;
#11480 = PRESENTATION_STYLE_ASSIGNMENT (( #6672 ) ) ;
#11481 = CARTESIAN_POINT ( 'NONE',  ( 10.00344141768317563, -22.05068747287765873, 5.250000000000000888 ) ) ;
#11482 = DIRECTION ( 'NONE',  ( 1.000000000000000000, 0.000000000000000000, 0.000000000000000000 ) ) ;
#11483 = CARTESIAN_POINT ( 'NONE',  ( -5.128441417683177406, -20.24999999999999289, 3.550687472877664952 ) ) ;
#11484 = VECTOR ( 'NONE', #15315, 1000.000000000000000 ) ;
#11485 = ORIENTED_EDGE ( 'NONE', *, *, #9934, .T. ) ;
#11486 = CARTESIAN_POINT ( 'NONE',  ( 10.65280858231679595, -20.91377862118960351, 5.979004561291660913 ) ) ;
#11487 = CARTESIAN_POINT ( 'NONE',  ( 12.62515553039088090, -20.24214571525854467, 4.629702272822510345 ) ) ;
#11488 = CARTESIAN_POINT ( 'NONE',  ( -13.11704875914858270, 3.848462337001107070, 6.754267079155989784 ) ) ;
#11489 = VERTEX_POINT ( 'NONE', #11561 ) ;
#11490 = CARTESIAN_POINT ( 'NONE',  ( -14.49999999999999645, -22.99999999999998579, 4.000000000000000000 ) ) ;
#11491 = LINE ( 'NONE', #17870, #3987 ) ;
#11492 = ORIENTED_EDGE ( 'NONE', *, *, #15494, .T. ) ;
#11493 = ORIENTED_EDGE ( 'NONE', *, *, #18347, .F. ) ;
#11494 = PLANE ( 'NONE',  #19836 ) ;
#11495 = AXIS2_PLACEMENT_3D ( 'NONE', #876, #15298, #1091 ) ;
#11496 = ORIENTED_EDGE ( 'NONE', *, *, #858, .T. ) ;
#11497 = CARTESIAN_POINT ( 'NONE',  ( -13.37155858231679595, -19.49999999999998934, 3.449312527122348371 ) ) ;
#11498 = EDGE_CURVE ( 'NONE', #19423, #14130, #6554, .T. ) ;
#11499 = CARTESIAN_POINT ( 'NONE',  ( 13.12529397354238192, 5.014845663890295846, 4.333333333333374782 ) ) ;
#11500 = CARTESIAN_POINT ( 'NONE',  ( 19.73630159782011617, 0.000000000000000000, 1.000000000000000000 ) ) ;
#11501 = EDGE_CURVE ( 'NONE', #10019, #9838, #1744, .T. ) ;
#11502 = CARTESIAN_POINT ( 'NONE',  ( 13.00900269284621302, -0.8578640112522492034, 5.903024842915844062 ) ) ;
#11503 = DIRECTION ( 'NONE',  ( 0.000000000000000000, 0.000000000000000000, 1.000000000000000000 ) ) ;
#11504 = CARTESIAN_POINT ( 'NONE',  ( -13.82811627091129836, 3.382371681020614584, 5.229645796715683304 ) ) ;
#11505 = CARTESIAN_POINT ( 'NONE',  ( 13.09030858231679417, -21.01515356694490322, 0.9790045612916562501 ) ) ;
#11506 = CARTESIAN_POINT ( 'NONE',  ( -13.11345185444515415, 3.666818649476655700, 6.750360829155977349 ) ) ;
#11507 = CARTESIAN_POINT ( 'NONE',  ( -6.621558582316796837, -24.50000000000000000, 3.550687472877651629 ) ) ;
#11508 = DIRECTION ( 'NONE',  ( 1.000000000000000000, 0.000000000000000000, -0.000000000000000000 ) ) ;
#11509 = FACE_OUTER_BOUND ( 'NONE', #12201, .T. ) ;
#11510 = CARTESIAN_POINT ( 'NONE',  ( 10.74655858231679595, -21.94931252712234127, 4.499999999999999112 ) ) ;
#11511 = CARTESIAN_POINT ( 'NONE',  ( -5.690941417683176518, -23.27327832286946219, 4.701595411283453707 ) ) ;
#11512 = VERTEX_POINT ( 'NONE', #14591 ) ;
#11513 = VERTEX_POINT ( 'NONE', #3610 ) ;
#11514 = CARTESIAN_POINT ( 'NONE',  ( 13.84501474873290938, 4.235744811019327649, 4.974109985360144037 ) ) ;
#11515 = CARTESIAN_POINT ( 'NONE',  ( -11.00000000000000000, -18.49999999999999645, 6.500000000000000888 ) ) ;
#11516 = VERTEX_POINT ( 'NONE', #3305 ) ;
#11517 = LINE ( 'NONE', #13185, #11136 ) ;
#11518 = LINE ( 'NONE', #15908, #18065 ) ;
#11519 = CARTESIAN_POINT ( 'NONE',  ( 13.39170256340046095, -19.40652054827866380, 5.481861153867630065 ) ) ;
#11520 = DIRECTION ( 'NONE',  ( 1.000000000000000000, 0.000000000000000000, -0.000000000000000000 ) ) ;
#11521 = CARTESIAN_POINT ( 'NONE',  ( 20.00000000000000000, -5.999999999999994671, 2.000000000000000000 ) ) ;
#11522 = EDGE_CURVE ( 'NONE', #10727, #9894, #18052, .T. ) ;
#11523 = CARTESIAN_POINT ( 'NONE',  ( 0.000000000000000000, -9.114917468222230923, 1.622643865078341019 ) ) ;
#11524 = VECTOR ( 'NONE', #18578, 1000.000000000000000 ) ;
#11525 = CARTESIAN_POINT ( 'NONE',  ( -12.66369984131459070, -18.29565801360988075, 5.528024842915327142 ) ) ;
#11526 = CARTESIAN_POINT ( 'NONE',  ( 6.902808582316795061, -22.77556120703056308, 1.770995438708340197 ) ) ;
#11527 = CARTESIAN_POINT ( 'NONE',  ( 14.49999999999999822, -23.00000000000001421, 1.000000000000000000 ) ) ;
#11528 = CARTESIAN_POINT ( 'NONE',  ( 13.06655316810189227, 2.048434989138931961, 5.965524842914772030 ) ) ;
#11529 = CARTESIAN_POINT ( 'NONE',  ( -1.337453470010121714, -9.864917468222230923, 2.372643865078341019 ) ) ;
#11530 = EDGE_CURVE ( 'NONE', #8356, #5395, #2149, .T. ) ;
#11531 = ADVANCED_FACE ( 'NONE', ( #266 ), #16373, .T. ) ;
#11532 = CARTESIAN_POINT ( 'NONE',  ( -13.87454419214980739, 4.976981703567351367, 5.131312659523921127 ) ) ;
#11533 = DIRECTION ( 'NONE',  ( 0.000000000000000000, 0.000000000000000000, 1.000000000000000000 ) ) ;
#11534 = CARTESIAN_POINT ( 'NONE',  ( 10.84719141768317563, -21.22443879296941915, 1.770995438708345748 ) ) ;
#11535 = CARTESIAN_POINT ( 'NONE',  ( -7.184058582316795949, -21.32873467460644079, 2.757051763020455404 ) ) ;
#11536 = VERTEX_POINT ( 'NONE', #16272 ) ;
#11537 = CARTESIAN_POINT ( 'NONE',  ( 12.62500000000002132, -20.99999999999450395, 3.833333333368183382 ) ) ;
#11538 = CARTESIAN_POINT ( 'NONE',  ( 12.64571531779736979, -19.20387645123237164, 5.508493592915143289 ) ) ;
#11539 = LINE ( 'NONE', #243, #8679 ) ;
#11540 = ORIENTED_EDGE ( 'NONE', *, *, #6925, .F. ) ;
#11541 = ORIENTED_EDGE ( 'NONE', *, *, #10873, .T. ) ;
#11542 = CARTESIAN_POINT ( 'NONE',  ( 7.499999999999999112, -24.49999999999999289, 5.000000000000000000 ) ) ;
#11543 = AXIS2_PLACEMENT_3D ( 'NONE', #7875, #9337, #10913 ) ;
#11544 = PLANE ( 'NONE',  #18252 ) ;
#11545 = LINE ( 'NONE', #16355, #1627 ) ;
#11546 = EDGE_CURVE ( 'NONE', #14385, #10351, #16059, .T. ) ;
#11547 = CARTESIAN_POINT ( 'NONE',  ( -20.00000000000000000, 0.000000000000000000, 1.000000000000000000 ) ) ;
#11548 = CARTESIAN_POINT ( 'NONE',  ( 2.049450250860079592, -10.15122911285664564, 1.696174415070213382 ) ) ;
#11549 = DIRECTION ( 'NONE',  ( 0.000000000000000000, 0.000000000000000000, 1.000000000000000000 ) ) ;
#11550 = DIRECTION ( 'NONE',  ( 0.000000000000000000, 1.000000000000000000, 0.000000000000000000 ) ) ;
#11551 = CARTESIAN_POINT ( 'NONE',  ( 12.62672070884157804, -20.24999999999983658, 3.550922209436377042 ) ) ;
#11552 = DIRECTION ( 'NONE',  ( -0.000000000000000000, -0.000000000000000000, -1.000000000000000000 ) ) ;
#11553 = CARTESIAN_POINT ( 'NONE',  ( -9.902808582316794173, -22.77556120703056308, 1.770995438708339975 ) ) ;
#11554 = CARTESIAN_POINT ( 'NONE',  ( -3.270401025279431995, -9.547343748290430199, 2.676314555138040063 ) ) ;
#11555 = VERTEX_POINT ( 'NONE', #6958 ) ;
#11556 = CARTESIAN_POINT ( 'NONE',  ( -12.62525331949183105, -19.48720736566255951, 4.581880915780448760 ) ) ;
#11557 = CARTESIAN_POINT ( 'NONE',  ( -5.496558582316795949, -22.05068747287764452, 2.499999999999999112 ) ) ;
#11558 = CARTESIAN_POINT ( 'NONE',  ( -10.19094141768317563, -23.27327832286946219, 4.701595411283453707 ) ) ;
#11559 = ORIENTED_EDGE ( 'NONE', *, *, #9741, .T. ) ;
#11560 = CARTESIAN_POINT ( 'NONE',  ( 13.74418849449709512, -0.8559810278826442964, 5.138499963383082125 ) ) ;
#11561 = CARTESIAN_POINT ( 'NONE',  ( -5.563547257480587760, 10.00000000000000000, 0.000000000000000000 ) ) ;
#11562 = VERTEX_POINT ( 'NONE', #2051 ) ;
#11563 = EDGE_CURVE ( 'NONE', #15857, #17187, #9686, .T. ) ;
#11564 = ORIENTED_EDGE ( 'NONE', *, *, #14477, .T. ) ;
#11565 = CARTESIAN_POINT ( 'NONE',  ( 0.000000000000000000, 10.00000000000000000, 1.000000000000000000 ) ) ;
#11566 = ORIENTED_EDGE ( 'NONE', *, *, #5555, .T. ) ;
#11567 = DIRECTION ( 'NONE',  ( -1.000000000000000000, -2.312964634635730039E-15, 0.000000000000000000 ) ) ;
#11568 = VERTEX_POINT ( 'NONE', #14493 ) ;
#11569 = CARTESIAN_POINT ( 'NONE',  ( 0.000000000000000000, 9.000000000000001776, 1.000000000000000000 ) ) ;
#11570 = DIRECTION ( 'NONE',  ( 1.000000000000000000, 0.000000000000000000, 0.000000000000000000 ) ) ;
#11571 = EDGE_CURVE ( 'NONE', #1689, #10727, #19320, .T. ) ;
#11572 = EDGE_CURVE ( 'NONE', #18339, #20096, #17746, .T. ) ;
#11573 = CARTESIAN_POINT ( 'NONE',  ( -13.87500000000000000, 4.995017896875348917, 3.999999999999998224 ) ) ;
#11574 = CARTESIAN_POINT ( 'NONE',  ( 11.00000000000000000, -19.49999999999999645, 5.000000000000000000 ) ) ;
#11575 = CARTESIAN_POINT ( 'NONE',  ( -8.027808582316792396, -23.72900456129165292, 4.275561207030568411 ) ) ;
#11576 = EDGE_CURVE ( 'NONE', #7093, #10351, #11465, .T. ) ;
#11577 = CARTESIAN_POINT ( 'NONE',  ( -22.81633994409548549, 0.000000000000000000, 0.000000000000000000 ) ) ;
#11578 = CARTESIAN_POINT ( 'NONE',  ( 10.19094141768317563, -23.27327832286946219, 4.701595411283453707 ) ) ;
#11579 = CARTESIAN_POINT ( 'NONE',  ( -13.49999999999998401, -19.49999999999999645, 4.000000000000000000 ) ) ;
#11580 = CARTESIAN_POINT ( 'NONE',  ( -4.097191417683176518, -22.77556120703057729, 5.229004561291655584 ) ) ;
#11581 = ORIENTED_EDGE ( 'NONE', *, *, #2552, .F. ) ;
#11582 = CARTESIAN_POINT ( 'NONE',  ( 10.84030858231679595, -22.98484643305508612, 6.020995438708344416 ) ) ;
#11583 = CARTESIAN_POINT ( 'NONE',  ( 13.10252221513633941, 3.864871864382954048, 6.004587342915129966 ) ) ;
#11584 = CARTESIAN_POINT ( 'NONE',  ( -13.12035191997235906, 4.015271958632619764, 6.757839745787993735 ) ) ;
#11585 = ORIENTED_EDGE ( 'NONE', *, *, #809, .F. ) ;
#11586 = EDGE_CURVE ( 'NONE', #19129, #9899, #8227, .T. ) ;
#11587 = CARTESIAN_POINT ( 'NONE',  ( 11.99178095869207006, 4.999999999999999112, 1.000000000000000000 ) ) ;
#11588 = CARTESIAN_POINT ( 'NONE',  ( 13.12499999999999645, 5.000000000000047073, 3.999999999999996447 ) ) ;
#11589 = ORIENTED_EDGE ( 'NONE', *, *, #7235, .F. ) ;
#11590 = CARTESIAN_POINT ( 'NONE',  ( 0.000000000000000000, 0.000000000000000000, 0.000000000000000000 ) ) ;
#11591 = VERTEX_POINT ( 'NONE', #17847 ) ;
#11592 = CARTESIAN_POINT ( 'NONE',  ( -0.000000000000000000, 10.00000000000000000, 0.000000000000000000 ) ) ;
#11593 = ORIENTED_EDGE ( 'NONE', *, *, #16019, .F. ) ;
#11594 = CARTESIAN_POINT ( 'NONE',  ( -20.49999999999998224, -21.99999999999999645, 9.999999999999998224 ) ) ;
#11595 = LINE ( 'NONE', #16409, #12611 ) ;
#11596 = LINE ( 'NONE', #10455, #2121 ) ;
#11597 = CARTESIAN_POINT ( 'NONE',  ( 12.62562019941893432, -20.21867992933967173, 4.757612834768309540 ) ) ;
#11598 = FACE_OUTER_BOUND ( 'NONE', #15931, .T. ) ;
#11599 = CIRCLE ( 'NONE', #6966, 0.3750000000000003331 ) ;
#11600 = CARTESIAN_POINT ( 'NONE',  ( 7.934058582316796837, -23.73192549717337130, 5.303608408759367343 ) ) ;
#11601 = CARTESIAN_POINT ( 'NONE',  ( -13.11862022235054503, 3.927821228673052723, 6.755987001683414483 ) ) ;
#11602 = CARTESIAN_POINT ( 'NONE',  ( -11.31594141768317741, -20.26807450282663225, 5.303608408759377113 ) ) ;
#11603 = CARTESIAN_POINT ( 'NONE',  ( -14.49999999999999645, -21.00000000000000355, 4.000000000000000000 ) ) ;
#11604 = CARTESIAN_POINT ( 'NONE',  ( -0.000000000000000000, 11.64110105645932691, 0.000000000000000000 ) ) ;
#11605 = EDGE_CURVE ( 'NONE', #3437, #7178, #14699, .T. ) ;
#11606 = CARTESIAN_POINT ( 'NONE',  ( 9.996558582316795949, -22.05068747287764452, 2.499999999999999112 ) ) ;
#11607 = CARTESIAN_POINT ( 'NONE',  ( -4.472191417683177406, -23.72900456129164937, 2.724438792969417378 ) ) ;
#11608 = VERTEX_POINT ( 'NONE', #13133 ) ;
#11609 = ORIENTED_EDGE ( 'NONE', *, *, #2665, .F. ) ;
#11610 = CARTESIAN_POINT ( 'NONE',  ( 13.39722611581222189, -19.12758115148224647, 5.495601574623241170 ) ) ;
#11611 = CARTESIAN_POINT ( 'NONE',  ( 4.750698171653723989, 11.64110105645932691, 10.00000000000000000 ) ) ;
#11612 = VERTEX_POINT ( 'NONE', #8325 ) ;
#11613 = PLANE ( 'NONE',  #5776 ) ;
#11614 = DIRECTION ( 'NONE',  ( -0.000000000000000000, -0.000000000000000000, -1.000000000000000000 ) ) ;
#11615 = VECTOR ( 'NONE', #10442, 1000.000000000000000 ) ;
#11616 = PLANE ( 'NONE',  #2956 ) ;
#11617 = CARTESIAN_POINT ( 'NONE',  ( 13.44218742460511073, -16.85703505742523234, 5.544429699623282914 ) ) ;
#11618 = DIRECTION ( 'NONE',  ( 0.000000000000000000, -1.000000000000000000, 0.000000000000000000 ) ) ;
#11619 = CARTESIAN_POINT ( 'NONE',  ( 0.2815691515810352930, -9.114917468222230923, 2.372643865078523984 ) ) ;
#11620 = CARTESIAN_POINT ( 'NONE',  ( -0.000000000000000000, 10.00000000000000000, 0.000000000000000000 ) ) ;
#11621 = CARTESIAN_POINT ( 'NONE',  ( -13.12529397354238192, 5.014845663890295846, 3.666666666666500873 ) ) ;
#11622 = CARTESIAN_POINT ( 'NONE',  ( 6.340308582316794173, -22.67418626127525982, 5.270995438708342640 ) ) ;
#11623 = LINE ( 'NONE', #3791, #2379 ) ;
#11624 = CARTESIAN_POINT ( 'NONE',  ( 12.64323021897839006, -19.32937394158751943, 5.504219675487169283 ) ) ;
#11625 = VECTOR ( 'NONE', #18797, 1000.000000000000000 ) ;
#11626 = CARTESIAN_POINT ( 'NONE',  ( -1.619022621591187150, -9.114917468222230923, 2.372643865078341019 ) ) ;
#11627 = CARTESIAN_POINT ( 'NONE',  ( 7.840308582316795949, -22.36352608949544418, 4.520995438708343528 ) ) ;
#11628 = CARTESIAN_POINT ( 'NONE',  ( 9.534691417683177406, -20.22900456129164581, 2.825813738724747726 ) ) ;
#11629 = CARTESIAN_POINT ( 'NONE',  ( -8.309058582316795949, -22.74294823697954016, 2.828734674606448785 ) ) ;
#11630 = ORIENTED_EDGE ( 'NONE', *, *, #18332, .F. ) ;
#11631 = CARTESIAN_POINT ( 'NONE',  ( 13.87005939078915873, 4.000499234880882327, 6.742989431566016378 ) ) ;
#11632 = CARTESIAN_POINT ( 'NONE',  ( 13.09532840572934376, 3.501584489333809724, 5.996774842915142401 ) ) ;
#11633 = DIRECTION ( 'NONE',  ( -0.000000000000000000, 0.000000000000000000, -1.000000000000000000 ) ) ;
#11634 = EDGE_LOOP ( 'NONE', ( #13687, #8660, #6580, #10644 ) ) ;
#11635 = EDGE_CURVE ( 'NONE', #4631, #16371, #14805, .T. ) ;
#11636 = ORIENTED_EDGE ( 'NONE', *, *, #14774, .T. ) ;
#11637 = LINE ( 'NONE', #18028, #102 ) ;
#11638 = DIRECTION ( 'NONE',  ( 1.000000000000000000, 0.000000000000000000, 0.000000000000000000 ) ) ;
#11639 = CIRCLE ( 'NONE', #16652, 10.00000000000000000 ) ;
#11640 = EDGE_CURVE ( 'NONE', #4975, #11436, #19730, .T. ) ;
#11641 = EDGE_CURVE ( 'NONE', #1443, #6686, #15003, .T. ) ;
#11642 = VECTOR ( 'NONE', #511, 1000.000000000000000 ) ;
#11643 = CARTESIAN_POINT ( 'NONE',  ( -26.19203811574920593, 0.000000000000000000, 0.000000000000000000 ) ) ;
#11644 = DIRECTION ( 'NONE',  ( 1.000000000000000000, 0.000000000000000000, 0.000000000000000000 ) ) ;
#11645 = CARTESIAN_POINT ( 'NONE',  ( 2.567175533087980188, -9.771398394011347577, 2.541241281345096859 ) ) ;
#11646 = LINE ( 'NONE', #8310, #16729 ) ;
#11647 = DIRECTION ( 'NONE',  ( -1.000000000000000000, -0.000000000000000000, -0.000000000000000000 ) ) ;
#11648 = DIRECTION ( 'NONE',  ( 0.000000000000000000, 0.000000000000000000, -1.000000000000000000 ) ) ;
#11649 = CARTESIAN_POINT ( 'NONE',  ( -5.381197846483055436, -14.00000000000000000, 2.000000000000000000 ) ) ;
#11650 = CARTESIAN_POINT ( 'NONE',  ( -10.18405858231679417, -20.79840458871652942, 2.226721677130544030 ) ) ;
#11651 = CARTESIAN_POINT ( 'NONE',  ( -3.321934647848983957, -9.834888441627915867, 2.750161776669472591 ) ) ;
#11652 = VERTEX_POINT ( 'NONE', #5391 ) ;
#11653 = CARTESIAN_POINT ( 'NONE',  ( -13.05202662408965075, 2.064844516520778939, 5.215845106673912213 ) ) ;
#11654 = CARTESIAN_POINT ( 'NONE',  ( -8.684058582316794173, -20.79840458871652942, 2.226721677130544030 ) ) ;
#11655 = CARTESIAN_POINT ( 'NONE',  ( -9.347191417683177406, -21.22443879296941915, 1.770995438708345748 ) ) ;
#11656 = VECTOR ( 'NONE', #3771, 1000.000000000000000 ) ;
#11657 = VERTEX_POINT ( 'NONE', #7381 ) ;
#11658 = CARTESIAN_POINT ( 'NONE',  ( 13.76337198624852398, 0.1127853055781036368, 5.159333296715827188 ) ) ;
#11659 = ORIENTED_EDGE ( 'NONE', *, *, #4045, .F. ) ;
#11660 = ORIENTED_EDGE ( 'NONE', *, *, #8519, .T. ) ;
#11661 = CARTESIAN_POINT ( 'NONE',  ( -13.50000000000000178, 5.000000000000047962, 2.000000000000000000 ) ) ;
#11662 = EDGE_CURVE ( 'NONE', #911, #18185, #5597, .T. ) ;
#11663 = ORIENTED_EDGE ( 'NONE', *, *, #17407, .F. ) ;
#11664 = CARTESIAN_POINT ( 'NONE',  ( -11.99999999999999822, -18.50000000000000355, 4.000000000000000000 ) ) ;
#11665 = EDGE_LOOP ( 'NONE', ( #10571, #5650, #17400, #676 ) ) ;
#11666 = CARTESIAN_POINT ( 'NONE',  ( 5.222191417683177406, -20.27099543870833998, 4.275561207030583510 ) ) ;
#11667 = DIRECTION ( 'NONE',  ( -1.000000000000000000, -0.000000000000000000, -0.000000000000000000 ) ) ;
#11668 = AXIS2_PLACEMENT_3D ( 'NONE', #19603, #16154, #11633 ) ;
#11669 = DIRECTION ( 'NONE',  ( 1.000000000000000000, 0.000000000000000000, 0.000000000000000000 ) ) ;
#11670 = DIRECTION ( 'NONE',  ( 1.000000000000000000, 6.938893903907222067E-15, 0.000000000000000000 ) ) ;
#11671 = CARTESIAN_POINT ( 'NONE',  ( -8.215308582316792396, -23.77099543870833998, 2.825813738724734847 ) ) ;
#11672 = AXIS2_PLACEMENT_3D ( 'NONE', #15891, #7945, #6391 ) ;
#11673 = DIRECTION ( 'NONE',  ( 0.000000000000000000, 1.000000000000000000, 0.000000000000000000 ) ) ;
#11674 = CARTESIAN_POINT ( 'NONE',  ( 8.409691417683177406, -21.32581373872474373, 5.270995438708348857 ) ) ;
#11675 = LINE ( 'NONE', #596, #9885 ) ;
#11676 = CARTESIAN_POINT ( 'NONE',  ( -5.409691417683178294, -21.63647391050456648, 4.520995438708348857 ) ) ;
#11677 = CARTESIAN_POINT ( 'NONE',  ( -7.840308582316795949, -22.98484643305508612, 6.020995438708344416 ) ) ;
#11678 = ORIENTED_EDGE ( 'NONE', *, *, #13895, .T. ) ;
#11679 = CARTESIAN_POINT ( 'NONE',  ( 12.65410809543883985, -18.78004118034163739, 5.517608176248461227 ) ) ;
#11680 = CARTESIAN_POINT ( 'NONE',  ( -13.10985494974158705, 3.485174961951963191, 6.746454579156001330 ) ) ;
#11681 = AXIS2_PLACEMENT_3D ( 'NONE', #615, #12879, #2183 ) ;
#11682 = ORIENTED_EDGE ( 'NONE', *, *, #2751, .T. ) ;
#11683 = DIRECTION ( 'NONE',  ( 1.000000000000000000, 0.000000000000000000, -0.000000000000000000 ) ) ;
#11684 = EDGE_CURVE ( 'NONE', #2297, #16697, #13634, .T. ) ;
#11685 = DIRECTION ( 'NONE',  ( 1.000000000000000000, -0.000000000000000000, 0.000000000000000000 ) ) ;
#11686 = PRESENTATION_LAYER_ASSIGNMENT (  '', '', ( #7696 ) ) ;
#11687 = ADVANCED_FACE ( 'NONE', ( #11967 ), #8632, .T. ) ;
#11688 = ORIENTED_EDGE ( 'NONE', *, *, #8398, .T. ) ;
#11689 = VERTEX_POINT ( 'NONE', #15112 ) ;
#11690 = VECTOR ( 'NONE', #438, 1000.000000000000000 ) ;
#11691 = CARTESIAN_POINT ( 'NONE',  ( 13.27375163337954156, -19.99368846338235883, 3.462660621537502870 ) ) ;
#11692 = ORIENTED_EDGE ( 'NONE', *, *, #15540, .F. ) ;
#11693 = DIRECTION ( 'NONE',  ( 1.000000000000000000, 0.000000000000000000, 0.000000000000000000 ) ) ;
#11694 = CARTESIAN_POINT ( 'NONE',  ( 13.12529418130016445, 5.014856155665242454, 4.958178834604180629 ) ) ;
#11695 = DIRECTION ( 'NONE',  ( 0.000000000000000000, 1.000000000000000000, 0.000000000000000000 ) ) ;
#11696 = CARTESIAN_POINT ( 'NONE',  ( -11.00000000000000000, -18.49999999999999645, 6.500000000000000888 ) ) ;
#11697 = VECTOR ( 'NONE', #18192, 1000.000000000000000 ) ;
#11698 = EDGE_CURVE ( 'NONE', #6312, #17224, #888, .T. ) ;
#11699 = CARTESIAN_POINT ( 'NONE',  ( 12.62499979224180180, -20.25001049178813162, 4.458178821399696012 ) ) ;
#11700 = CYLINDRICAL_SURFACE ( 'NONE', #18383, 10.00000000000000000 ) ;
#11701 = AXIS2_PLACEMENT_3D ( 'NONE', #8912, #5979, #16951 ) ;
#11702 = CARTESIAN_POINT ( 'NONE',  ( 10.27780858231679595, -19.52099543870833642, 2.413778621189609286 ) ) ;
#11703 = CARTESIAN_POINT ( 'NONE',  ( -13.14782865898149034, 5.402847278557675104, 6.092770214907355708 ) ) ;
#11704 = VECTOR ( 'NONE', #11357, 1000.000000000000000 ) ;
#11705 = CARTESIAN_POINT ( 'NONE',  ( -6.340308582316796837, -22.98484643305508612, 6.020995438708344416 ) ) ;
#11706 = VECTOR ( 'NONE', #11854, 1000.000000000000000 ) ;
#11707 = LINE ( 'NONE', #5441, #12615 ) ;
#11708 = DIRECTION ( 'NONE',  ( 1.000000000000000000, 0.000000000000000000, 0.000000000000000000 ) ) ;
#11709 = CARTESIAN_POINT ( 'NONE',  ( 9.902808582316795949, -22.46490103525074034, 2.520995438708341307 ) ) ;
#11710 = EDGE_CURVE ( 'NONE', #10231, #10101, #2452, .T. ) ;
#11711 = DIRECTION ( 'NONE',  ( 0.000000000000000000, 0.5000000000000037748, -0.8660254037844365982 ) ) ;
#11712 = ORIENTED_EDGE ( 'NONE', *, *, #17369, .F. ) ;
#11713 = EDGE_CURVE ( 'NONE', #6020, #8442, #19840, .T. ) ;
#11714 = ORIENTED_EDGE ( 'NONE', *, *, #19303, .T. ) ;
#11715 = CARTESIAN_POINT ( 'NONE',  ( 13.44218742460511073, -16.85703505742523234, 5.544429699623282914 ) ) ;
#11716 = DIRECTION ( 'NONE',  ( -1.000000000000000000, 0.000000000000000000, 0.000000000000000000 ) ) ;
#11717 = CARTESIAN_POINT ( 'NONE',  ( 22.56633994409548194, 0.000000000000000000, 1.000000000000000000 ) ) ;
#11718 = ORIENTED_EDGE ( 'NONE', *, *, #2498, .T. ) ;
#11719 = DIRECTION ( 'NONE',  ( 3.469446951953611033E-15, -1.000000000000000000, 0.000000000000000000 ) ) ;
#11720 = AXIS2_PLACEMENT_3D ( 'NONE', #17888, #16117, #13074 ) ;
#11721 = CARTESIAN_POINT ( 'NONE',  ( 0.000000000000000000, 4.999999999999999112, 1.000000000000000000 ) ) ;
#11722 = DIRECTION ( 'NONE',  ( 1.000000000000000000, 0.000000000000000000, 0.000000000000000000 ) ) ;
#11723 = VECTOR ( 'NONE', #7883, 1000.000000000000000 ) ;
#11724 = CARTESIAN_POINT ( 'NONE',  ( 13.85528666703740619, 4.004476685417483139, 5.993048563355776182 ) ) ;
#11725 = VECTOR ( 'NONE', #13502, 1000.000000000000000 ) ;
#11726 = VECTOR ( 'NONE', #6557, 1000.000000000000000 ) ;
#11727 = FACE_OUTER_BOUND ( 'NONE', #12539, .T. ) ;
#11728 = CARTESIAN_POINT ( 'NONE',  ( 1.619022621591186928, -8.364917468222230923, 2.372643865078341019 ) ) ;
#11729 = ADVANCED_FACE ( 'NONE', ( #18157 ), #18259, .T. ) ;
#11730 = DIRECTION ( 'NONE',  ( 0.000000000000000000, 0.000000000000000000, -1.000000000000000000 ) ) ;
#11731 = CARTESIAN_POINT ( 'NONE',  ( -12.63598464672302590, -18.94527534048458151, 4.764022190007618285 ) ) ;
#11732 = CARTESIAN_POINT ( 'NONE',  ( 9.340308582316794173, -22.67418626127525982, 5.270995438708342640 ) ) ;
#11733 = LINE ( 'NONE', #3575, #6062 ) ;
#11734 = CARTESIAN_POINT ( 'NONE',  ( 12.65410809543883985, -18.78004118034163739, 5.517608176248461227 ) ) ;
#11735 = CARTESIAN_POINT ( 'NONE',  ( -2.583953725994688533, -9.847075946378776479, 2.560676788604062004 ) ) ;
#11736 = CARTESIAN_POINT ( 'NONE',  ( 10.93405858231679595, -22.67126532539354855, 4.242948236979545484 ) ) ;
#11737 = VECTOR ( 'NONE', #6945, 1000.000000000000000 ) ;
#11738 = CARTESIAN_POINT ( 'NONE',  ( 8.503441417683177406, -22.05068747287765873, 5.250000000000000888 ) ) ;
#11739 = CARTESIAN_POINT ( 'NONE',  ( -5.121558582316795061, -22.99999999999999645, 3.550687472877652073 ) ) ;
#11740 = ORIENTED_EDGE ( 'NONE', *, *, #12802, .T. ) ;
#11741 = CARTESIAN_POINT ( 'NONE',  ( 13.12519991495504712, 4.260095705229160146, 6.739971950528219402 ) ) ;
#11742 = CARTESIAN_POINT ( 'NONE',  ( 13.09358652029869141, 4.163619275088517035, 5.207983256689002083 ) ) ;
#11743 = CARTESIAN_POINT ( 'NONE',  ( -12.62672070884157804, -20.24999999999991473, 3.550922209436377042 ) ) ;
#11744 = ORIENTED_EDGE ( 'NONE', *, *, #11198, .F. ) ;
#11745 = EDGE_LOOP ( 'NONE', ( #7252, #3420, #296, #9532 ) ) ;
#11746 = FACE_OUTER_BOUND ( 'NONE', #10468, .T. ) ;
#11747 = DIRECTION ( 'NONE',  ( -0.000000000000000000, 1.000000000000000000, 0.000000000000000000 ) ) ;
#11748 = DIRECTION ( 'NONE',  ( 0.000000000000000000, 1.000000000000000000, -0.000000000000000000 ) ) ;
#11749 = VECTOR ( 'NONE', #12226, 1000.000000000000000 ) ;
#11750 = CARTESIAN_POINT ( 'NONE',  ( -21.42243175760212637, 4.999999999999999112, 1.000000000000000000 ) ) ;
#11751 = CARTESIAN_POINT ( 'NONE',  ( 2.702705060698113115, -10.69015907548275379, 2.777197378435510622 ) ) ;
#11752 = CARTESIAN_POINT ( 'NONE',  ( 13.12500000000000178, 5.000000000000047962, 4.000000000000000000 ) ) ;
#11753 = DIRECTION ( 'NONE',  ( 0.000000000000000000, 1.000000000000000000, -0.000000000000000000 ) ) ;
#11754 = EDGE_CURVE ( 'NONE', #8919, #4928, #4028, .T. ) ;
#11755 = CARTESIAN_POINT ( 'NONE',  ( 13.23120918948287361, -20.54541409651599082, 3.468569357888747540 ) ) ;
#11756 = CARTESIAN_POINT ( 'NONE',  ( -2.592143777221601386, -9.905122062175031772, 2.575584190728205325 ) ) ;
#11757 = CARTESIAN_POINT ( 'NONE',  ( -5.121558582316794173, -23.74999999999999645, 3.550687472877651629 ) ) ;
#11758 = CARTESIAN_POINT ( 'NONE',  ( -1.407845757905374695, -8.364917468222230923, 2.372643865078341019 ) ) ;
#11759 = ORIENTED_EDGE ( 'NONE', *, *, #11903, .F. ) ;
#11760 = CARTESIAN_POINT ( 'NONE',  ( -13.09560264576187905, 4.265433610975056133, 3.666666666666500873 ) ) ;
#11761 = CARTESIAN_POINT ( 'NONE',  ( -6.715308582316794173, -23.77099543870833998, 2.825813738724734847 ) ) ;
#11762 = CARTESIAN_POINT ( 'NONE',  ( -5.878441417683177406, -23.74999999999999645, 3.449312527122335492 ) ) ;
#11763 = ORIENTED_EDGE ( 'NONE', *, *, #10270, .T. ) ;
#11764 = CARTESIAN_POINT ( 'NONE',  ( 13.37499999999998579, -20.24999999999999289, 3.146526952850934755 ) ) ;
#11765 = DIRECTION ( 'NONE',  ( -8.673617379884047798E-17, 1.000000000000000000, -0.000000000000000000 ) ) ;
#11766 = ORIENTED_EDGE ( 'NONE', *, *, #3855, .T. ) ;
#11767 = ORIENTED_EDGE ( 'NONE', *, *, #5453, .T. ) ;
#11768 = VECTOR ( 'NONE', #14573, 1000.000000000000000 ) ;
#11769 = FACE_OUTER_BOUND ( 'NONE', #7222, .T. ) ;
#11770 = VERTEX_POINT ( 'NONE', #10201 ) ;
#11771 = CARTESIAN_POINT ( 'NONE',  ( -24.87918902992234393, 11.64110105645932691, 0.000000000000000000 ) ) ;
#11772 = ORIENTED_EDGE ( 'NONE', *, *, #3366, .F. ) ;
#11773 = PLANE ( 'NONE',  #10672 ) ;
#11774 = CARTESIAN_POINT ( 'NONE',  ( -15.49999999999999822, -20.99999999999999645, 4.000000000000000000 ) ) ;
#11775 = CARTESIAN_POINT ( 'NONE',  ( -15.11404127825609223, 9.000000000000001776, 1.000000000000000000 ) ) ;
#11776 = CARTESIAN_POINT ( 'NONE',  ( 0.2815691515810352930, -9.114917468222230923, 2.372643865078523984 ) ) ;
#11777 = CARTESIAN_POINT ( 'NONE',  ( -7.934058582316792396, -23.20159541128345992, 4.773278322869455970 ) ) ;
#11778 = VECTOR ( 'NONE', #9747, 1000.000000000000000 ) ;
#11779 = EDGE_CURVE ( 'NONE', #9991, #346, #18469, .T. ) ;
#11780 = CARTESIAN_POINT ( 'NONE',  ( 13.87144757537903494, 4.070602556641903291, 6.741633940066556363 ) ) ;
#11781 = LINE ( 'NONE', #6873, #17979 ) ;
#11782 = CARTESIAN_POINT ( 'NONE',  ( 10.19094141768317741, -22.74294823697955081, 4.171265325393542334 ) ) ;
#11783 = CARTESIAN_POINT ( 'NONE',  ( -12.64195242771744709, -19.39390240027112000, 5.496549442168085164 ) ) ;
#11784 = CARTESIAN_POINT ( 'NONE',  ( -7.472191417683177406, -22.97900456129165292, 3.035098964749240125 ) ) ;
#11785 = CARTESIAN_POINT ( 'NONE',  ( -6.246558582316795949, -21.94931252712234127, 6.000000000000001776 ) ) ;
#11786 = ORIENTED_EDGE ( 'NONE', *, *, #11433, .T. ) ;
#11787 = EDGE_CURVE ( 'NONE', #7606, #8680, #2554, .T. ) ;
#11788 = CARTESIAN_POINT ( 'NONE',  ( 13.10557919622060652, 4.019249409169220577, 6.007898877577752650 ) ) ;
#11789 = CARTESIAN_POINT ( 'NONE',  ( -13.09546733092777160, 2.758600211853326822, 6.730829579156167419 ) ) ;
#11790 = ORIENTED_EDGE ( 'NONE', *, *, #1913, .T. ) ;
#11791 = ADVANCED_FACE ( 'NONE', ( #2246 ), #2662, .T. ) ;
#11792 = CARTESIAN_POINT ( 'NONE',  ( 22.56633994409548194, 0.000000000000000000, 0.000000000000000000 ) ) ;
#11793 = CARTESIAN_POINT ( 'NONE',  ( 0.000000000000000000, -0.5000000000000004441, 0.5000000000000000000 ) ) ;
#11794 = VECTOR ( 'NONE', #10344, 1000.000000000000000 ) ;
#11795 = EDGE_LOOP ( 'NONE', ( #11036, #6985, #1892, #12827 ) ) ;
#11796 = ORIENTED_EDGE ( 'NONE', *, *, #1174, .F. ) ;
#11797 = CARTESIAN_POINT ( 'NONE',  ( 13.29909190252318041, -20.02341932109202105, 3.459266583615586033 ) ) ;
#11798 = ORIENTED_EDGE ( 'NONE', *, *, #7276, .F. ) ;
#11799 = DIRECTION ( 'NONE',  ( -0.1351665943404306014, -0.9596796555888912339, 0.2464649070825229438 ) ) ;
#11800 = CARTESIAN_POINT ( 'NONE',  ( 12.69247507894198712, -16.84250851341299082, 5.559274842915185033 ) ) ;
#11801 = CARTESIAN_POINT ( 'NONE',  ( -3.342893013439646843, -9.383962644129466568, 1.884355023724047173 ) ) ;
#11802 = LINE ( 'NONE', #2705, #5311 ) ;
#11803 = PLANE ( 'NONE',  #6465 ) ;
#11804 = ADVANCED_FACE ( 'NONE', ( #15420 ), #3921, .F. ) ;
#11805 = VECTOR ( 'NONE', #8881, 1000.000000000000000 ) ;
#11806 = CARTESIAN_POINT ( 'NONE',  ( 13.12529397354238192, 5.014845663890295846, 4.666666666666619889 ) ) ;
#11807 = CARTESIAN_POINT ( 'NONE',  ( 4.413027396565882832, -21.64511906963072363, 4.828480566969830079 ) ) ;
#11808 = CARTESIAN_POINT ( 'NONE',  ( 10.09030858231679595, -21.01515356694490322, 0.9790045612916562501 ) ) ;
#11809 = CARTESIAN_POINT ( 'NONE',  ( -13.15498530132288479, 5.764257716805535559, 2.999999999999999556 ) ) ;
#11810 = CARTESIAN_POINT ( 'NONE',  ( -4.190941417683176518, -23.80360840875937001, 5.231925497173365081 ) ) ;
#11811 = VERTEX_POINT ( 'NONE', #13537 ) ;
#11812 = LINE ( 'NONE', #3659, #19100 ) ;
#11813 = CARTESIAN_POINT ( 'NONE',  ( 9.715308582316795949, -23.02099543870833998, 3.136473910504556262 ) ) ;
#11814 = DIRECTION ( 'NONE',  ( -0.000000000000000000, 0.000000000000000000, -1.000000000000000000 ) ) ;
#11815 = ORIENTED_EDGE ( 'NONE', *, *, #12092, .F. ) ;
#11816 = ORIENTED_EDGE ( 'NONE', *, *, #17948, .T. ) ;
#11817 = CARTESIAN_POINT ( 'NONE',  ( 13.39482594849551944, -19.24878960097397140, 5.493002502378098839 ) ) ;
#11818 = CIRCLE ( 'NONE', #18853, 10.00000000000000000 ) ;
#11819 = CARTESIAN_POINT ( 'NONE',  ( -5.933390479346035029, 9.000000000000001776, 0.000000000000000000 ) ) ;
#11820 =( NAMED_UNIT ( * ) SI_UNIT ( $, .STERADIAN. ) SOLID_ANGLE_UNIT ( ) );
#11821 = EDGE_LOOP ( 'NONE', ( #2150, #3611, #11078, #20124, #6258, #14614 ) ) ;
#11822 = EDGE_CURVE ( 'NONE', #11689, #14392, #19741, .T. ) ;
#11823 = DIRECTION ( 'NONE',  ( -0.000000000000000000, -0.000000000000000000, -1.000000000000000000 ) ) ;
#11824 = CARTESIAN_POINT ( 'NONE',  ( 19.73630159782011617, 0.000000000000000000, 0.000000000000000000 ) ) ;
#11825 = DIRECTION ( 'NONE',  ( -0.000000000000000000, 1.000000000000000000, -0.000000000000000000 ) ) ;
#11826 = CARTESIAN_POINT ( 'NONE',  ( 13.39359219590679295, -19.31109410670777038, 5.491647114909025795 ) ) ;
#11827 = LINE ( 'NONE', #8806, #10200 ) ;
#11828 = CARTESIAN_POINT ( 'NONE',  ( 1.932703420524435112, -8.381852853175612239, 2.376993210252662969 ) ) ;
#11829 = EDGE_CURVE ( 'NONE', #10647, #3720, #5492, .T. ) ;
#11830 = EDGE_CURVE ( 'NONE', #13, #12186, #15212, .T. ) ;
#11831 = CARTESIAN_POINT ( 'NONE',  ( 0.9854920305337621089, -9.114917468222230923, 1.622643865078341463 ) ) ;
#11832 = CARTESIAN_POINT ( 'NONE',  ( -12.63238774201960268, -19.12691902800888499, 4.760115940007608515 ) ) ;
#11833 = CARTESIAN_POINT ( 'NONE',  ( 6.059058582316793284, -20.72672167713054137, 4.701595411283463477 ) ) ;
#11834 = DIRECTION ( 'NONE',  ( 0.000000000000000000, 1.000000000000000000, -0.000000000000000000 ) ) ;
#11835 = CARTESIAN_POINT ( 'NONE',  ( 12.62888984277510218, -20.05356293986039873, 5.111704976569332537 ) ) ;
#11836 = CARTESIAN_POINT ( 'NONE',  ( -2.567175533087980188, -9.771398394011347577, 2.541241281345096859 ) ) ;
#11837 = CARTESIAN_POINT ( 'NONE',  ( 7.934058582316796837, -22.67126532539354855, 4.242948236979545484 ) ) ;
#11838 = CARTESIAN_POINT ( 'NONE',  ( 7.847191417683176518, -21.22443879296941915, 1.770995438708345748 ) ) ;
#11839 = CARTESIAN_POINT ( 'NONE',  ( -8.121558582316792396, -23.74999999999999645, 3.550687472877651629 ) ) ;
#11840 = ORIENTED_EDGE ( 'NONE', *, *, #18715, .F. ) ;
#11841 = CARTESIAN_POINT ( 'NONE',  ( 13.15047398821051239, 5.536436404627260721, 5.896317606305554015 ) ) ;
#11842 = CARTESIAN_POINT ( 'NONE',  ( 12.63958155142659834, -18.76363165295958524, 4.767928440007602298 ) ) ;
#11843 = CARTESIAN_POINT ( 'NONE',  ( 27.00000000000000000, 0.000000000000000000, 1.000000000000000000 ) ) ;
#11844 = ORIENTED_EDGE ( 'NONE', *, *, #5199, .F. ) ;
#11845 = EDGE_CURVE ( 'NONE', #17, #17043, #20461, .T. ) ;
#11846 = VECTOR ( 'NONE', #12903, 1000.000000000000000 ) ;
#11847 = VERTEX_POINT ( 'NONE', #9556 ) ;
#11848 = CARTESIAN_POINT ( 'NONE',  ( -15.11404127825609223, 9.000000000000001776, 1.000000000000000000 ) ) ;
#11849 = CARTESIAN_POINT ( 'NONE',  ( 5.000000000000000000, -12.50000000000000000, 4.500000000000000888 ) ) ;
#11850 = DIRECTION ( 'NONE',  ( 0.000000000000000000, 0.000000000000000000, -1.000000000000000000 ) ) ;
#11851 = CARTESIAN_POINT ( 'NONE',  ( -3.944195004867014909, -21.61378581760806128, 5.207602947182413011 ) ) ;
#11852 = CARTESIAN_POINT ( 'NONE',  ( 1.797604806073912709, -9.120796646272857799, 2.374153755450133740 ) ) ;
#11853 = CARTESIAN_POINT ( 'NONE',  ( 19.73630159782011617, 9.000000000000001776, 1.000000000000000000 ) ) ;
#11854 = DIRECTION ( 'NONE',  ( -0.000000000000000000, -0.000000000000000000, -1.000000000000000000 ) ) ;
#11855 = CARTESIAN_POINT ( 'NONE',  ( -26.94203811574920593, 10.00000000000000000, 0.000000000000000000 ) ) ;
#11856 = DIRECTION ( 'NONE',  ( 0.000000000000000000, 1.000000000000000000, 0.000000000000000000 ) ) ;
#11857 = CARTESIAN_POINT ( 'NONE',  ( -7.559058582316794173, -20.72672167713054137, 4.701595411283463477 ) ) ;
#11858 = CARTESIAN_POINT ( 'NONE',  ( -3.292205091070697698, -9.639507599131205140, 2.699984073191874057 ) ) ;
#11859 = ORIENTED_EDGE ( 'NONE', *, *, #5958, .T. ) ;
#11860 = CARTESIAN_POINT ( 'NONE',  ( -13.37505992445764136, -19.49697381488866554, 4.539006848837218833 ) ) ;
#11861 = CARTESIAN_POINT ( 'NONE',  ( -8.590308582316794173, -21.32581373872472597, 1.729004561291657582 ) ) ;
#11862 = CARTESIAN_POINT ( 'NONE',  ( -3.944195004867016241, -21.61378581760806838, 5.207602947182413899 ) ) ;
#11863 = ORIENTED_EDGE ( 'NONE', *, *, #12533, .F. ) ;
#11864 = CARTESIAN_POINT ( 'NONE',  ( 13.84983662433050178, 3.729249528687784920, 5.987138032956566214 ) ) ;
#11866 = CARTESIAN_POINT ( 'NONE',  ( 15.86404127825609400, 0.000000000000000000, 0.000000000000000000 ) ) ;
#11865 = CIRCLE ( 'NONE', #8189, 10.00000000000000000 ) ;
#11867 = ORIENTED_EDGE ( 'NONE', *, *, #14265, .T. ) ;
#11868 = PRESENTATION_LAYER_ASSIGNMENT (  '', '', ( #14541 ) ) ;
#11869 = ORIENTED_EDGE ( 'NONE', *, *, #19487, .T. ) ;
#11870 = ADVANCED_FACE ( 'NONE', ( #17292 ), #18780, .F. ) ;
#11871 = PLANE ( 'NONE',  #4424 ) ;
#11872 = ORIENTED_EDGE ( 'NONE', *, *, #19336, .F. ) ;
#11873 = DIRECTION ( 'NONE',  ( -0.000000000000000000, -0.000000000000000000, -1.000000000000000000 ) ) ;
#11874 = EDGE_LOOP ( 'NONE', ( #10954, #5447 ) ) ;
#11875 = CARTESIAN_POINT ( 'NONE',  ( 5.972191417683177406, -23.72900456129164937, 2.724438792969417378 ) ) ;
#11876 = CARTESIAN_POINT ( 'NONE',  ( -26.04469207716614321, -2.255140518769849223E-14, 1.000000000000000000 ) ) ;
#11877 = CARTESIAN_POINT ( 'NONE',  ( 14.49999999999998579, -21.99999999999999645, 12.00000000000000355 ) ) ;
#11878 = CARTESIAN_POINT ( 'NONE',  ( 0.000000000000000000, -9.114917468222230923, 2.372643865078340575 ) ) ;
#11879 = PLANE ( 'NONE',  #9309 ) ;
#11880 = CARTESIAN_POINT ( 'NONE',  ( 12.62499999999998224, -20.99999999999998934, 4.166666666666637653 ) ) ;
#11881 = FACE_OUTER_BOUND ( 'NONE', #10075, .T. ) ;
#11882 = CARTESIAN_POINT ( 'NONE',  ( 12.44094141768317741, -21.25705176302044208, 2.828734674606458555 ) ) ;
#11883 = CARTESIAN_POINT ( 'NONE',  ( -12.63943061533661982, -19.52125392549825733, 5.470334935344855154 ) ) ;
#11884 = CARTESIAN_POINT ( 'NONE',  ( -4.284691417683177406, -23.02099543870834353, 3.863526089495429972 ) ) ;
#11885 = CARTESIAN_POINT ( 'NONE',  ( -7.378441417683177406, -24.50000000000000000, 3.449312527122335048 ) ) ;
#11886 = ORIENTED_EDGE ( 'NONE', *, *, #2254, .F. ) ;
#11887 = CARTESIAN_POINT ( 'NONE',  ( 13.12529397354238192, 5.014845663890295846, 3.000000000000000000 ) ) ;
#11888 = CARTESIAN_POINT ( 'NONE',  ( -13.10252221513633941, 3.864871864382954048, 6.004587342915129966 ) ) ;
#11889 = VERTEX_POINT ( 'NONE', #18984 ) ;
#11890 = CARTESIAN_POINT ( 'NONE',  ( -15.61404127825609223, 9.000000000000001776, 1.000000000000000000 ) ) ;
#11891 = CARTESIAN_POINT ( 'NONE',  ( 20.00000000000000000, -5.999999999999994671, 2.000000000000000000 ) ) ;
#11892 =( BOUNDED_CURVE ( )  B_SPLINE_CURVE ( 3, ( #1542, #8138, #17538, #18816 ),
 .UNSPECIFIED., .F., .F. ) 
 B_SPLINE_CURVE_WITH_KNOTS ( ( 4, 4 ),
 ( 1.119769514998634197, 1.570796326794896558 ),
 .UNSPECIFIED. ) 
 CURVE ( )  GEOMETRIC_REPRESENTATION_ITEM ( )  RATIONAL_B_SPLINE_CURVE ( ( 1.000000000000000000, 0.9831196229872642967, 0.9831196229872642967, 1.000000000000000000 ) ) 
 REPRESENTATION_ITEM ( '' )  );
#11893 = ORIENTED_EDGE ( 'NONE', *, *, #12459, .T. ) ;
#11894 = ORIENTED_EDGE ( 'NONE', *, *, #14069, .F. ) ;
#11895 = EDGE_CURVE ( 'NONE', #13440, #5494, #4640, .T. ) ;
#11896 = VERTEX_POINT ( 'NONE', #2974 ) ;
#11897 = FACE_OUTER_BOUND ( 'NONE', #19481, .T. ) ;
#11898 = CARTESIAN_POINT ( 'NONE',  ( 13.10557919622060652, 4.019249409169220577, 6.007898877577752650 ) ) ;
#11899 = EDGE_CURVE ( 'NONE', #10437, #6147, #13944, .T. ) ;
#11900 = CARTESIAN_POINT ( 'NONE',  ( -2.844469389063872811, -10.54053385813977606, 1.988770633557972012 ) ) ;
#11901 = DIRECTION ( 'NONE',  ( 1.000000000000000000, 6.938893903907232322E-16, -0.000000000000000000 ) ) ;
#11902 = DIRECTION ( 'NONE',  ( -0.000000000000000000, -0.000000000000000000, -1.000000000000000000 ) ) ;
#11903 = EDGE_CURVE ( 'NONE', #19625, #18278, #5905, .T. ) ;
#11904 = CARTESIAN_POINT ( 'NONE',  ( 0.000000000000000000, 9.000000000000001776, 1.000000000000000000 ) ) ;
#11905 = DIRECTION ( 'NONE',  ( -0.000000000000000000, -0.000000000000000000, -1.000000000000000000 ) ) ;
#11906 = CARTESIAN_POINT ( 'NONE',  ( 9.628441417683177406, -19.49999999999998934, 3.550687472877664952 ) ) ;
#11907 = CARTESIAN_POINT ( 'NONE',  ( -12.64195242771744709, -19.39390240027112000, 5.496549442168085164 ) ) ;
#11908 = CARTESIAN_POINT ( 'NONE',  ( -8.409691417683177406, -21.01515356694492098, 6.020995438708349745 ) ) ;
#11909 = ORIENTED_EDGE ( 'NONE', *, *, #4015, .F. ) ;
#11910 = DIRECTION ( 'NONE',  ( -1.000000000000000000, 0.000000000000000000, 0.000000000000000000 ) ) ;
#11911 = FACE_OUTER_BOUND ( 'NONE', #9627, .T. ) ;
#11912 = CARTESIAN_POINT ( 'NONE',  ( -13.86833701876684088, 3.913519447696059750, 6.741146579470268740 ) ) ;
#11913 = CARTESIAN_POINT ( 'NONE',  ( 6.621558582316796837, -22.99999999999999645, 3.550687472877652073 ) ) ;
#11914 = DIRECTION ( 'NONE',  ( 1.000000000000000000, 0.000000000000000000, 0.000000000000000000 ) ) ;
#11915 = ORIENTED_EDGE ( 'NONE', *, *, #10029, .F. ) ;
#11916 = ORIENTED_EDGE ( 'NONE', *, *, #13115, .F. ) ;
#11917 = CARTESIAN_POINT ( 'NONE',  ( 13.87406079471522347, 4.952570133121557028, 5.260711232101737522 ) ) ;
#11918 = LINE ( 'NONE', #6812, #3421 ) ;
#11919 =( LENGTH_UNIT ( ) NAMED_UNIT ( * ) SI_UNIT ( .MILLI., .METRE. ) );
#11920 = ORIENTED_EDGE ( 'NONE', *, *, #14564, .T. ) ;
#11921 = ADVANCED_FACE ( 'NONE', ( #20247 ), #3182, .T. ) ;
#11922 = DIRECTION ( 'NONE',  ( -0.8660254037844417052, 0.4999999999999947264, 0.000000000000000000 ) ) ;
#11923 = AXIS2_PLACEMENT_3D ( 'NONE', #18841, #20106, #13804 ) ;
#11924 = PLANE ( 'NONE',  #11048 ) ;
#11925 = DIRECTION ( 'NONE',  ( 0.000000000000000000, -0.000000000000000000, 1.000000000000000000 ) ) ;
#11926 = CARTESIAN_POINT ( 'NONE',  ( 13.40022353639839103, -18.97621141187856608, 5.498856782956575984 ) ) ;
#11927 = FACE_OUTER_BOUND ( 'NONE', #17563, .T. ) ;
#11928 = CARTESIAN_POINT ( 'NONE',  ( 1.619022621591187150, -9.114917468222230923, 2.372643865078341019 ) ) ;
#11929 = DIRECTION ( 'NONE',  ( -0.000000000000000000, -0.000000000000000000, -1.000000000000000000 ) ) ;
#11930 = CARTESIAN_POINT ( 'NONE',  ( -12.62868952012632207, -19.31367923361656480, 4.748088538831167327 ) ) ;
#11931 = LINE ( 'NONE', #18325, #19334 ) ;
#11932 = CARTESIAN_POINT ( 'NONE',  ( 11.68405858231679417, -20.79840458871652942, 2.226721677130544030 ) ) ;
#11933 = CARTESIAN_POINT ( 'NONE',  ( -13.84517967659089521, 2.744073667841084418, 6.715984435864265301 ) ) ;
#11934 = EDGE_CURVE ( 'NONE', #19548, #13158, #9351, .T. ) ;
#11935 = LINE ( 'NONE', #3994, #17381 ) ;
#11936 = CARTESIAN_POINT ( 'NONE',  ( 8.590308582316797725, -21.63647391050454871, 2.479004561291657804 ) ) ;
#11937 = CARTESIAN_POINT ( 'NONE',  ( 8.034691417683175629, -20.22900456129164581, 2.825813738724747726 ) ) ;
#11938 = CARTESIAN_POINT ( 'NONE',  ( -12.71530858231679240, -23.77099543870833998, 2.825813738724734847 ) ) ;
#11939 = ORIENTED_EDGE ( 'NONE', *, *, #3383, .T. ) ;
#11940 = CARTESIAN_POINT ( 'NONE',  ( 13.15316049959406364, 5.672105229501871904, 5.573635960501007958 ) ) ;
#11941 = CARTESIAN_POINT ( 'NONE',  ( 13.06641424290328501, 2.791419266617020334, 5.231470106674447784 ) ) ;
#11942 = CARTESIAN_POINT ( 'NONE',  ( -5.933390479346035029, 0.000000000000000000, 1.000000000000000000 ) ) ;
#11943 = ORIENTED_EDGE ( 'NONE', *, *, #7312, .F. ) ;
#11944 = EDGE_CURVE ( 'NONE', #5816, #9416, #7581, .T. ) ;
#11945 = EDGE_LOOP ( 'NONE', ( #16782, #14512, #9327, #8459 ) ) ;
#11946 = EDGE_CURVE ( 'NONE', #510, #15982, #2872, .T. ) ;
#11947 = CARTESIAN_POINT ( 'NONE',  ( 0.000000000000000000, 16.00000000000000000, 1.000000000000000000 ) ) ;
#11948 = DIRECTION ( 'NONE',  ( 1.000000000000000000, 0.000000000000000000, 0.000000000000000000 ) ) ;
#11949 = CARTESIAN_POINT ( 'NONE',  ( -5.000000000000000000, -12.50000000000000000, 4.500000000000000888 ) ) ;
#11950 = VECTOR ( 'NONE', #7924, 1000.000000000000000 ) ;
#11951 = FACE_OUTER_BOUND ( 'NONE', #2897, .T. ) ;
#11952 = CARTESIAN_POINT ( 'NONE',  ( 2.513306525444908512, -9.622685169956881168, 2.503048754562789746 ) ) ;
#11953 = DIRECTION ( 'NONE',  ( 0.000000000000000000, 1.000000000000000000, 0.000000000000000000 ) ) ;
#11954 = DIRECTION ( 'NONE',  ( -0.000000000000000000, -0.000000000000000000, 1.000000000000000000 ) ) ;
#11955 = VECTOR ( 'NONE', #10859, 1000.000000000000000 ) ;
#11956 = CARTESIAN_POINT ( 'NONE',  ( 2.499999999999998668, -19.50000000000000000, 1.000000000000000000 ) ) ;
#11957 = CARTESIAN_POINT ( 'NONE',  ( -2.583953725994688533, -9.847075946378776479, 2.560676788604062004 ) ) ;
#11958 = CARTESIAN_POINT ( 'NONE',  ( -4.840308582316793284, -22.67418626127525982, 5.270995438708342640 ) ) ;
#11959 = CARTESIAN_POINT ( 'NONE',  ( -3.564229130755586006, -10.39902496812945465, 2.145043306434553987 ) ) ;
#11960 = EDGE_LOOP ( 'NONE', ( #7612, #20201, #2128, #16616, #4876 ) ) ;
#11961 = CARTESIAN_POINT ( 'NONE',  ( -13.38007464613909470, -19.24373036997283037, 4.743072998953621777 ) ) ;
#11962 = CARTESIAN_POINT ( 'NONE',  ( -7.465308582316795061, -20.22900456129164937, 4.174186261275266929 ) ) ;
#11963 = CARTESIAN_POINT ( 'NONE',  ( 12.62155858231679417, -24.50000000000000000, 3.550687472877651629 ) ) ;
#11964 = CARTESIAN_POINT ( 'NONE',  ( -11.97219141768317918, -22.97900456129165292, 3.035098964749240125 ) ) ;
#11965 = VERTEX_POINT ( 'NONE', #9249 ) ;
#11966 = CARTESIAN_POINT ( 'NONE',  ( 13.85403523778986390, 3.941279508358651817, 5.991705257707216958 ) ) ;
#11967 = FACE_OUTER_BOUND ( 'NONE', #15788, .T. ) ;
#11968 = ORIENTED_EDGE ( 'NONE', *, *, #19488, .T. ) ;
#11969 = ORIENTED_EDGE ( 'NONE', *, *, #608, .T. ) ;
#11970 = LINE ( 'NONE', #10515, #13703 ) ;
#11971 = AXIS2_PLACEMENT_3D ( 'NONE', #13392, #16626, #15268 ) ;
#11972 = ORIENTED_EDGE ( 'NONE', *, *, #9611, .F. ) ;
#11973 = ADVANCED_FACE ( 'NONE', ( #4339 ), #8425, .F. ) ;
#11974 = CARTESIAN_POINT ( 'NONE',  ( -13.37741471237955260, -20.12805702483293757, 4.993653275319895890 ) ) ;
#11975 = VERTEX_POINT ( 'NONE', #5924 ) ;
#11976 = DIRECTION ( 'NONE',  ( -0.000000000000000000, -0.000000000000000000, -1.000000000000000000 ) ) ;
#11977 = CARTESIAN_POINT ( 'NONE',  ( 5.000000000000000000, -7.500000000000000000, 1.000000000000000000 ) ) ;
#11978 = DIRECTION ( 'NONE',  ( 0.000000000000000000, 0.000000000000000000, 1.000000000000000000 ) ) ;
#11979 = AXIS2_PLACEMENT_3D ( 'NONE', #8541, #14912, #7083 ) ;
#11980 = CARTESIAN_POINT ( 'NONE',  ( 3.422464802389687311, -10.54865018547243061, 2.933470051312085936 ) ) ;
#11981 = CARTESIAN_POINT ( 'NONE',  ( -4.840308582316793284, -22.67418626127525982, 5.270995438708342640 ) ) ;
#11982 = AXIS2_PLACEMENT_3D ( 'NONE', #16282, #19329, #276 ) ;
#11983 = EDGE_CURVE ( 'NONE', #4521, #9180, #12295, .T. ) ;
#11984 = CARTESIAN_POINT ( 'NONE',  ( 12.63178515739782348, -20.65734955141111584, 5.567013446834313761 ) ) ;
#11985 = CIRCLE ( 'NONE', #18363, 10.00000000000000000 ) ;
#11986 = CARTESIAN_POINT ( 'NONE',  ( 24.62918902992234038, 0.000000000000000000, 0.000000000000000000 ) ) ;
#11987 = VECTOR ( 'NONE', #6153, 1000.000000000000000 ) ;
#11988 = CARTESIAN_POINT ( 'NONE',  ( 5.972191417683179182, -23.72900456129165292, 2.724438792969417822 ) ) ;
#11989 = DIRECTION ( 'NONE',  ( -0.000000000000000000, -0.000000000000000000, -1.000000000000000000 ) ) ;
#11990 = CARTESIAN_POINT ( 'NONE',  ( -8.222191417683175629, -21.02099543870834353, 3.964901035250761208 ) ) ;
#11991 = CARTESIAN_POINT ( 'NONE',  ( -11.78469141768317741, -24.52099543870834708, 4.484846433055073689 ) ) ;
#11992 = ORIENTED_EDGE ( 'NONE', *, *, #5534, .T. ) ;
#11993 = CARTESIAN_POINT ( 'NONE',  ( 13.12529418130016445, 5.014856155665242454, 4.958178834604180629 ) ) ;
#11994 = CARTESIAN_POINT ( 'NONE',  ( -12.91308523408712183, -5.701695678577235249, 5.798858176249892082 ) ) ;
#11995 = ORIENTED_EDGE ( 'NONE', *, *, #3355, .F. ) ;
#11996 = CARTESIAN_POINT ( 'NONE',  ( -11.00000000000000000, -19.49999999999999645, 4.000000000000000000 ) ) ;
#11997 = DIRECTION ( 'NONE',  ( -1.000000000000000000, -0.000000000000000000, -0.000000000000000000 ) ) ;
#11998 = EDGE_LOOP ( 'NONE', ( #14928, #19431, #15874, #9603 ) ) ;
#11999 = CIRCLE ( 'NONE', #12665, 0.4999999999999987232 ) ;
#12000 = AXIS2_PLACEMENT_3D ( 'NONE', #11876, #2563, #12088 ) ;
#12001 = CONTEXT_DEPENDENT_SHAPE_REPRESENTATION ( #18025, #9508 ) ;
#12002 = ORIENTED_EDGE ( 'NONE', *, *, #9260, .F. ) ;
#12003 = AXIS2_PLACEMENT_3D ( 'NONE', #12361, #14225, #6289 ) ;
#12004 = ORIENTED_EDGE ( 'NONE', *, *, #12469, .T. ) ;
#12005 = CARTESIAN_POINT ( 'NONE',  ( 10.00000000000000533, -30.00000000000000355, 1.000000000000000000 ) ) ;
#12006 = CARTESIAN_POINT ( 'NONE',  ( -17.94064177244175795, 0.000000000000000000, 0.000000000000000000 ) ) ;
#12007 = CARTESIAN_POINT ( 'NONE',  ( -3.436477319925839602, -9.631595465688135960, 1.947952079262935676 ) ) ;
#12008 = FACE_OUTER_BOUND ( 'NONE', #5276, .T. ) ;
#12009 = DIRECTION ( 'NONE',  ( -3.469446951953611033E-15, 1.000000000000000000, 0.000000000000000000 ) ) ;
#12010 = CARTESIAN_POINT ( 'NONE',  ( -15.49999999999999822, -20.99999999999999645, 1.000000000000000000 ) ) ;
#12011 = CARTESIAN_POINT ( 'NONE',  ( 6.527808582316795949, -24.47900456129166358, 4.586221378810390270 ) ) ;
#12012 = CARTESIAN_POINT ( 'NONE',  ( -13.12529397354238192, 5.014845663890295846, 4.791666666666685614 ) ) ;
#12013 = CARTESIAN_POINT ( 'NONE',  ( -8.503441417683177406, -22.05068747287766229, 6.000000000000001776 ) ) ;
#12014 = CIRCLE ( 'NONE', #13035, 0.3749999999999997224 ) ;
#12015 = ORIENTED_EDGE ( 'NONE', *, *, #19901, .T. ) ;
#12016 = CARTESIAN_POINT ( 'NONE',  ( -6.313547257480587760, 0.000000000000000000, 1.000000000000000000 ) ) ;
#12017 = CARTESIAN_POINT ( 'NONE',  ( 0.000000000000000000, 11.64110105645932691, 10.00000000000000000 ) ) ;
#12018 = CARTESIAN_POINT ( 'NONE',  ( -13.67732412376249052, -5.732631749971324631, 6.533692769198849781 ) ) ;
#12019 = CIRCLE ( 'NONE', #19710, 1.000000000000002665 ) ;
#12020 = CARTESIAN_POINT ( 'NONE',  ( 11.49655858231679417, -22.05068747287764452, 1.749999999999998446 ) ) ;
#12021 = CARTESIAN_POINT ( 'NONE',  ( 11.00000000000000000, -18.49999999999999645, 6.500000000000000888 ) ) ;
#12022 = VERTEX_POINT ( 'NONE', #7402 ) ;
#12023 = ORIENTED_EDGE ( 'NONE', *, *, #1060, .T. ) ;
#12024 = CARTESIAN_POINT ( 'NONE',  ( 13.87470602645761986, 4.985154336109792972, 4.166666666666765551 ) ) ;
#12025 = PLANE ( 'NONE',  #18496 ) ;
#12026 = ORIENTED_EDGE ( 'NONE', *, *, #8173, .F. ) ;
#12027 = LINE ( 'NONE', #7440, #9131 ) ;
#12028 = VECTOR ( 'NONE', #15248, 1000.000000000000000 ) ;
#12029 = LINE ( 'NONE', #5659, #2025 ) ;
#12030 = DIRECTION ( 'NONE',  ( 1.000000000000000000, 0.000000000000000000, 0.000000000000000000 ) ) ;
#12031 = CARTESIAN_POINT ( 'NONE',  ( 0.000000000000000000, 9.000000000000001776, 1.000000000000000000 ) ) ;
#12032 = VECTOR ( 'NONE', #2811, 1000.000000000000000 ) ;
#12033 =( GEOMETRIC_REPRESENTATION_CONTEXT ( 3 ) GLOBAL_UNCERTAINTY_ASSIGNED_CONTEXT ( ( #20539 ) ) GLOBAL_UNIT_ASSIGNED_CONTEXT ( ( #17046, #20716, #12747 ) ) REPRESENTATION_CONTEXT ( 'NONE', 'WORKASPACE' ) );
#12034 = CARTESIAN_POINT ( 'NONE',  ( -5.563547257480587760, 0.000000000000000000, 1.000000000000000000 ) ) ;
#12035 = CARTESIAN_POINT ( 'NONE',  ( 1.337453470010121714, -9.114917468222230923, 2.372643865078341019 ) ) ;
#12036 = AXIS2_PLACEMENT_3D ( 'NONE', #4965, #14376, #8313 ) ;
#12037 = CARTESIAN_POINT ( 'NONE',  ( 27.94203811574922725, 3.231447299068595019E-14, 1.000000000000000000 ) ) ;
#12038 = CARTESIAN_POINT ( 'NONE',  ( -13.12529397354238192, 5.014845663890295846, 4.833333333333344584 ) ) ;
#12039 = PLANE ( 'NONE',  #17645 ) ;
#12040 = CARTESIAN_POINT ( 'NONE',  ( -19.48630159782011262, 4.999999999999999112, 0.000000000000000000 ) ) ;
#12041 = CARTESIAN_POINT ( 'NONE',  ( -13.40653076352726103, -19.40769644187082932, 6.236886054669082746 ) ) ;
#12042 = EDGE_CURVE ( 'NONE', #17483, #16676, #14072, .T. ) ;
#12043 = DIRECTION ( 'NONE',  ( -0.000000000000000000, -0.000000000000000000, -1.000000000000000000 ) ) ;
#12044 = CARTESIAN_POINT ( 'NONE',  ( 10.93405858231679417, -23.20159541128345992, 4.773278322869455970 ) ) ;
#12045 = CARTESIAN_POINT ( 'NONE',  ( 12.44094141768317741, -21.25705176302044208, 2.828734674606458555 ) ) ;
#12046 = CARTESIAN_POINT ( 'NONE',  ( -11.21530858231679417, -23.77099543870833998, 2.825813738724734847 ) ) ;
#12047 = VERTEX_POINT ( 'NONE', #13763 ) ;
#12048 = CARTESIAN_POINT ( 'NONE',  ( 12.64802275499843454, -19.83735087257960927, 6.157588447769994922 ) ) ;
#12049 = EDGE_CURVE ( 'NONE', #19600, #7153, #4148, .T. ) ;
#12050 = CARTESIAN_POINT ( 'NONE',  ( 12.63238774201960268, -19.12691902800888499, 4.760115940007608515 ) ) ;
#12051 = ADVANCED_FACE ( 'NONE', ( #18487 ), #7598, .F. ) ;
#12052 = CARTESIAN_POINT ( 'NONE',  ( 7.499999999999999112, -23.83493649053891517, 4.999999999999999112 ) ) ;
#12053 = VECTOR ( 'NONE', #14902, 1000.000000000000000 ) ;
#12054 = VERTEX_POINT ( 'NONE', #20167 ) ;
#12055 = AXIS2_PLACEMENT_3D ( 'NONE', #16463, #8311, #16658 ) ;
#12056 = VECTOR ( 'NONE', #15914, 1000.000000000000000 ) ;
#12057 = VERTEX_POINT ( 'NONE', #9168 ) ;
#12058 = CARTESIAN_POINT ( 'NONE',  ( -7.869520639128047002, 9.000000000000001776, 1.000000000000000000 ) ) ;
#12059 = VECTOR ( 'NONE', #19826, 1000.000000000000000 ) ;
#12060 = CARTESIAN_POINT ( 'NONE',  ( -12.62515553039088090, -20.24214571525854467, 4.629702272822510345 ) ) ;
#12061 = CARTESIAN_POINT ( 'NONE',  ( -27.00000000000000000, 3.000000000000000000, 0.000000000000000000 ) ) ;
#12062 = LINE ( 'NONE', #4323, #6663 ) ;
#12063 = CARTESIAN_POINT ( 'NONE',  ( 0.5631383031621635116, -9.864917468222230923, 2.372643865078341019 ) ) ;
#12064 = CARTESIAN_POINT ( 'NONE',  ( 0.000000000000000000, 9.000000000000001776, 1.000000000000000000 ) ) ;
#12065 = AXIS2_PLACEMENT_3D ( 'NONE', #7855, #10897, #6501 ) ;
#12066 = DIRECTION ( 'NONE',  ( 1.000000000000000000, 0.000000000000000000, 0.000000000000000000 ) ) ;
#12067 = EDGE_CURVE ( 'NONE', #4874, #1688, #15541, .T. ) ;
#12068 = DIRECTION ( 'NONE',  ( 1.000000000000000000, 0.000000000000000000, -0.000000000000000000 ) ) ;
#12069 = CARTESIAN_POINT ( 'NONE',  ( -9.902808582316795949, -23.08622137881038938, 1.020995438708339309 ) ) ;
#12070 = CARTESIAN_POINT ( 'NONE',  ( -2.787023586469211001, -10.13267000451481614, 1.884023048047904103 ) ) ;
#12071 = ORIENTED_EDGE ( 'NONE', *, *, #8983, .F. ) ;
#12072 = CARTESIAN_POINT ( 'NONE',  ( -13.76337198624852398, 0.1127853055781036368, 5.159333296715827188 ) ) ;
#12073 = CARTESIAN_POINT ( 'NONE',  ( -7.090308582316794173, -21.32581373872472597, 1.729004561291657582 ) ) ;
#12074 = CARTESIAN_POINT ( 'NONE',  ( 11.97219141768317918, -24.47900456129165292, 2.413778621189595963 ) ) ;
#12075 = CARTESIAN_POINT ( 'NONE',  ( -10.84719141768317741, -21.53509896474923835, 2.520995438708346192 ) ) ;
#12076 = ORIENTED_EDGE ( 'NONE', *, *, #796, .T. ) ;
#12077 = CARTESIAN_POINT ( 'NONE',  ( 13.81626551376501588, 2.033908445126689557, 5.950679699622869911 ) ) ;
#12078 = CARTESIAN_POINT ( 'NONE',  ( 10.93924542913430820, 10.00000000000000000, 1.000000000000000000 ) ) ;
#12079 = ORIENTED_EDGE ( 'NONE', *, *, #10896, .T. ) ;
#12080 = VERTEX_POINT ( 'NONE', #5827 ) ;
#12081 = CARTESIAN_POINT ( 'NONE',  ( 6.063547257480584207, 10.00000000000000000, 1.000000000000000000 ) ) ;
#12082 = VERTEX_POINT ( 'NONE', #903 ) ;
#12083 = CARTESIAN_POINT ( 'NONE',  ( -13.83065313257865370, 2.760483195222930952, 5.966304699623404595 ) ) ;
#12084 = ADVANCED_FACE ( 'NONE', ( #12194 ), #20062, .T. ) ;
#12085 = AXIS2_PLACEMENT_3D ( 'NONE', #13791, #18517, #7320 ) ;
#12086 = ORIENTED_EDGE ( 'NONE', *, *, #12158, .T. ) ;
#12087 = PLANE ( 'NONE',  #20228 ) ;
#12088 = DIRECTION ( 'NONE',  ( -8.673617379884033500E-16, 1.000000000000000000, 0.000000000000000000 ) ) ;
#12089 = DIRECTION ( 'NONE',  ( 0.000000000000000000, 0.000000000000000000, 1.000000000000000000 ) ) ;
#12090 = CARTESIAN_POINT ( 'NONE',  ( 3.292205091070697698, -9.639507599131205140, 2.699984073191874057 ) ) ;
#12091 = CARTESIAN_POINT ( 'NONE',  ( -14.00000000000000000, 0.000000000000000000, 1.000000000000000000 ) ) ;
#12092 = EDGE_CURVE ( 'NONE', #19648, #15034, #1125, .T. ) ;
#12093 = CARTESIAN_POINT ( 'NONE',  ( 13.90258797164900884, 5.643192568275169130, 5.568788873356017355 ) ) ;
#12094 = DIRECTION ( 'NONE',  ( 0.000000000000000000, 0.000000000000000000, -1.000000000000000000 ) ) ;
#12095 = CARTESIAN_POINT ( 'NONE',  ( 25.37918902992234393, 11.64110105645932691, 10.00000000000000000 ) ) ;
#12096 = EDGE_CURVE ( 'NONE', #13635, #18461, #9069, .T. ) ;
#12097 = DIRECTION ( 'NONE',  ( 1.000000000000000000, 0.000000000000000000, 0.000000000000000000 ) ) ;
#12098 = CARTESIAN_POINT ( 'NONE',  ( 9.909691417683175629, -21.63647391050456648, 4.520995438708348857 ) ) ;
#12099 = CARTESIAN_POINT ( 'NONE',  ( 10.93924542913430820, 0.000000000000000000, 0.000000000000000000 ) ) ;
#12100 = CARTESIAN_POINT ( 'NONE',  ( -3.944195004867014909, -21.80034658733847053, 4.481176709221804444 ) ) ;
#12101 = VECTOR ( 'NONE', #5287, 1000.000000000000000 ) ;
#12102 = CARTESIAN_POINT ( 'NONE',  ( -11.59719141768317741, -23.08622137881040359, 5.979004561291654696 ) ) ;
#12103 = ORIENTED_EDGE ( 'NONE', *, *, #15279, .F. ) ;
#12104 = CARTESIAN_POINT ( 'NONE',  ( 12.72590726430969532, -14.40418315237199742, 4.861678440007700885 ) ) ;
#12105 = CARTESIAN_POINT ( 'NONE',  ( -12.64691428603184242, -19.14332855539073464, 5.509795676248469221 ) ) ;
#12106 = ORIENTED_EDGE ( 'NONE', *, *, #13242, .T. ) ;
#12107 = DIRECTION ( 'NONE',  ( -1.000000000000000000, 0.000000000000000000, 0.000000000000000000 ) ) ;
#12108 = LINE ( 'NONE', #3947, #4988 ) ;
#12109 = ORIENTED_EDGE ( 'NONE', *, *, #19139, .T. ) ;
#12110 = VERTEX_POINT ( 'NONE', #7503 ) ;
#12111 = ADVANCED_FACE ( 'NONE', ( #12505 ), #15229, .F. ) ;
#12112 = ORIENTED_EDGE ( 'NONE', *, *, #19216, .F. ) ;
#12113 = DIRECTION ( 'NONE',  ( 0.000000000000000000, 1.000000000000000000, -0.000000000000000000 ) ) ;
#12114 = VECTOR ( 'NONE', #3779, 1000.000000000000000 ) ;
#12115 = DIRECTION ( 'NONE',  ( 0.000000000000000000, 0.000000000000000000, 1.000000000000000000 ) ) ;
#12116 = CARTESIAN_POINT ( 'NONE',  ( -2.012076196476103362, -9.160103213191565175, 1.634248467062433541 ) ) ;
#12117 = DIRECTION ( 'NONE',  ( 0.000000000000000000, -1.000000000000000000, 0.000000000000000000 ) ) ;
#12118 = CARTESIAN_POINT ( 'NONE',  ( 14.49999999999998579, -19.52007894294123957, 12.00000000000000000 ) ) ;
#12119 = DIRECTION ( 'NONE',  ( -0.000000000000000000, -0.000000000000000000, -1.000000000000000000 ) ) ;
#12120 = CARTESIAN_POINT ( 'NONE',  ( 9.722191417683177406, -19.52099543870834353, 4.586221378810406257 ) ) ;
#12121 = CARTESIAN_POINT ( 'NONE',  ( -13.10192273101908000, 3.834597916462216816, 6.003936301248457674 ) ) ;
#12122 = CARTESIAN_POINT ( 'NONE',  ( -6.253441417683175629, -21.94931252712233061, 0.9999999999999978906 ) ) ;
#12123 = ORIENTED_EDGE ( 'NONE', *, *, #6304, .T. ) ;
#12124 = CARTESIAN_POINT ( 'NONE',  ( 13.18405858231679417, -20.79840458871652942, 2.226721677130544030 ) ) ;
#12125 = DIRECTION ( 'NONE',  ( -0.000000000000000000, -0.000000000000000000, -1.000000000000000000 ) ) ;
#12126 = CARTESIAN_POINT ( 'NONE',  ( -13.86676110481170632, 3.833935792988865110, 6.739421935864088553 ) ) ;
#12127 = VECTOR ( 'NONE', #20614, 1000.000000000000000 ) ;
#12128 = CARTESIAN_POINT ( 'NONE',  ( 10.18405858231679417, -20.79840458871652942, 2.226721677130544030 ) ) ;
#12129 = CARTESIAN_POINT ( 'NONE',  ( -3.944195004867014909, -21.61378581760806128, 5.207602947182413011 ) ) ;
#12130 = ORIENTED_EDGE ( 'NONE', *, *, #661, .T. ) ;
#12131 = ORIENTED_EDGE ( 'NONE', *, *, #7829, .T. ) ;
#12132 = CARTESIAN_POINT ( 'NONE',  ( 13.38795836133016870, -20.34560275282643005, 5.879540349057044146 ) ) ;
#12133 = LINE ( 'NONE', #18731, #2783 ) ;
#12134 = ORIENTED_EDGE ( 'NONE', *, *, #1239, .T. ) ;
#12135 = EDGE_CURVE ( 'NONE', #10019, #2700, #7012, .T. ) ;
#12136 = CARTESIAN_POINT ( 'NONE',  ( 15.86404127825609400, 9.000000000000001776, 1.000000000000000000 ) ) ;
#12137 = ORIENTED_EDGE ( 'NONE', *, *, #4541, .T. ) ;
#12138 = CARTESIAN_POINT ( 'NONE',  ( -9.621558582316794173, -23.74999999999999645, 3.550687472877651629 ) ) ;
#12139 = DIRECTION ( 'NONE',  ( 0.000000000000000000, -0.000000000000000000, 1.000000000000000000 ) ) ;
#12140 = AXIS2_PLACEMENT_3D ( 'NONE', #8261, #6589, #13165 ) ;
#12141 = CARTESIAN_POINT ( 'NONE',  ( 7.499999999999999112, -18.49999999999999645, 4.000000000000000000 ) ) ;
#12142 = CARTESIAN_POINT ( 'NONE',  ( 2.801385037117921861, -10.23463596792102415, 1.910209944425432349 ) ) ;
#12143 = DIRECTION ( 'NONE',  ( -1.000000000000000000, 0.000000000000000000, 0.000000000000000000 ) ) ;
#12144 = CARTESIAN_POINT ( 'NONE',  ( -13.37499999999998401, -19.49999999999998934, 3.146526952850934755 ) ) ;
#12145 = DIRECTION ( 'NONE',  ( -0.000000000000000000, 0.000000000000000000, -1.000000000000000000 ) ) ;
#12146 = CARTESIAN_POINT ( 'NONE',  ( -13.86833701876684088, 3.913519447696059750, 6.741146579470268740 ) ) ;
#12147 = FACE_OUTER_BOUND ( 'NONE', #16304, .T. ) ;
#12148 = CARTESIAN_POINT ( 'NONE',  ( 5.777808582316795949, -21.02099543870833998, 3.035098964749253003 ) ) ;
#12149 = CARTESIAN_POINT ( 'NONE',  ( 10.75344141768317741, -21.94931252712233061, 2.499999999999999112 ) ) ;
#12150 = CARTESIAN_POINT ( 'NONE',  ( -9.059058582316794173, -20.72672167713054137, 4.701595411283463477 ) ) ;
#12151 = ORIENTED_EDGE ( 'NONE', *, *, #10426, .T. ) ;
#12152 = CARTESIAN_POINT ( 'NONE',  ( 12.62506359033936754, -19.49678868786235597, 4.541393094775662220 ) ) ;
#12153 = LINE ( 'NONE', #10697, #13343 ) ;
#12154 = EDGE_LOOP ( 'NONE', ( #17429, #17222, #15572, #9661 ) ) ;
#12155 = UNCERTAINTY_MEASURE_WITH_UNIT (LENGTH_MEASURE( 1.000000000000000082E-05 ), #6380, 'distance_accuracy_value', 'NONE');
#12156 = ORIENTED_EDGE ( 'NONE', *, *, #17610, .F. ) ;
#12157 = PLANE ( 'NONE',  #6103 ) ;
#12158 = EDGE_CURVE ( 'NONE', #11516, #2248, #18902, .T. ) ;
#12159 = CARTESIAN_POINT ( 'NONE',  ( -12.62499999999998224, -20.24999999999998934, 4.166666666666636765 ) ) ;
#12160 = DIRECTION ( 'NONE',  ( -0.000000000000000000, -0.000000000000000000, -1.000000000000000000 ) ) ;
#12161 = CARTESIAN_POINT ( 'NONE',  ( -13.85528666703740619, 4.004476685417483139, 5.993048563355776182 ) ) ;
#12162 = EDGE_CURVE ( 'NONE', #19, #14460, #2996, .T. ) ;
#12163 = DIRECTION ( 'NONE',  ( 0.000000000000000000, 0.000000000000000000, 1.000000000000000000 ) ) ;
#12164 = PLANE ( 'NONE',  #10203 ) ;
#12165 = LINE ( 'NONE', #5690, #13491 ) ;
#12166 = EDGE_CURVE ( 'NONE', #8796, #15857, #9678, .T. ) ;
#12167 = CARTESIAN_POINT ( 'NONE',  ( 25.04469207716615031, 9.000000000000001776, 0.000000000000000000 ) ) ;
#12168 = CARTESIAN_POINT ( 'NONE',  ( -0.9854920305337621089, -9.114917468222230923, 2.372643865078341019 ) ) ;
#12169 = CARTESIAN_POINT ( 'NONE',  ( -8.871558582316795949, -19.49999999999998934, 3.449312527122348371 ) ) ;
#12170 = CARTESIAN_POINT ( 'NONE',  ( -1.619022621591186928, -8.364917468222230923, 1.622643865078341907 ) ) ;
#12171 = ORIENTED_EDGE ( 'NONE', *, *, #13999, .T. ) ;
#12172 = CARTESIAN_POINT ( 'NONE',  ( -13.42766088059286922, -16.84062553004338625, 4.794749963382423985 ) ) ;
#12173 = DIRECTION ( 'NONE',  ( -0.000000000000000000, -0.000000000000000000, -1.000000000000000000 ) ) ;
#12174 = CARTESIAN_POINT ( 'NONE',  ( 11.40969141768317918, -21.01515356694492098, 6.020995438708349745 ) ) ;
#12175 = CARTESIAN_POINT ( 'NONE',  ( -9.815941417683177406, -21.32873467460645145, 4.242948236979555254 ) ) ;
#12176 = VERTEX_POINT ( 'NONE', #10531 ) ;
#12177 = CARTESIAN_POINT ( 'NONE',  ( 13.66279757975024722, -5.716222222589476765, 5.784013032957989964 ) ) ;
#12178 = CARTESIAN_POINT ( 'NONE',  ( 11.00000000000000000, -24.49999999999999289, 5.000000000000000000 ) ) ;
#12179 = EDGE_LOOP ( 'NONE', ( #7516, #11160, #11593, #5362 ) ) ;
#12180 = EDGE_LOOP ( 'NONE', ( #18701, #18020, #20200, #11909 ) ) ;
#12181 = PLANE ( 'NONE',  #4737 ) ;
#12182 = VERTEX_POINT ( 'NONE', #19211 ) ;
#12183 = CARTESIAN_POINT ( 'NONE',  ( -13.87470623115321899, 4.985164673244912414, 4.958488177337359026 ) ) ;
#12184 = EDGE_CURVE ( 'NONE', #9402, #2930, #14380, .T. ) ;
#12185 = CARTESIAN_POINT ( 'NONE',  ( 2.513306525444908512, -9.622685169956881168, 2.503048754562789746 ) ) ;
#12186 = VERTEX_POINT ( 'NONE', #7905 ) ;
#12187 = CARTESIAN_POINT ( 'NONE',  ( -12.50209451496117197, 10.00000000000000000, 1.000000000000000000 ) ) ;
#12188 = CARTESIAN_POINT ( 'NONE',  ( -13.49999999999998401, -18.49999999999999645, 4.000000000000000000 ) ) ;
#12189 = CARTESIAN_POINT ( 'NONE',  ( 3.722205087890566144, -11.52065056559861134, 2.433099166587254558 ) ) ;
#12190 = CARTESIAN_POINT ( 'NONE',  ( 9.000000000000000000, -9.999999999999991118, 1.000000000000000000 ) ) ;
#12191 = CARTESIAN_POINT ( 'NONE',  ( 13.09546733092777160, 2.758600211853326822, 6.730829579156167419 ) ) ;
#12192 = CARTESIAN_POINT ( 'NONE',  ( 3.944195004867014909, -21.61378581760806128, 5.207602947182413011 ) ) ;
#12193 = DIRECTION ( 'NONE',  ( 0.000000000000000000, -1.000000000000000000, 0.000000000000000000 ) ) ;
#12194 = FACE_OUTER_BOUND ( 'NONE', #3391, .T. ) ;
#12195 = VECTOR ( 'NONE', #9949, 1000.000000000000000 ) ;
#12196 = VECTOR ( 'NONE', #16195, 1000.000000000000000 ) ;
#12197 = CARTESIAN_POINT ( 'NONE',  ( 10.75344141768317741, -21.94931252712233061, 2.499999999999999112 ) ) ;
#12198 = CARTESIAN_POINT ( 'NONE',  ( -25.29469207716615031, 4.999999999999999112, 1.000000000000000000 ) ) ;
#12199 = CARTESIAN_POINT ( 'NONE',  ( -9.434058582316795949, -22.67126532539354855, 4.242948236979545484 ) ) ;
#12200 = CARTESIAN_POINT ( 'NONE',  ( -9.065941417683177406, -23.73192549717336064, 1.696391591240623331 ) ) ;
#12201 = EDGE_LOOP ( 'NONE', ( #3341, #15210, #17753, #6602 ) ) ;
#12202 = CARTESIAN_POINT ( 'NONE',  ( 12.62499994688180749, -19.50000268246798640, 4.473800639250938183 ) ) ;
#12203 = CARTESIAN_POINT ( 'NONE',  ( -13.10431844137356627, 3.955581289335645234, 6.006545679920360925 ) ) ;
#12204 = EDGE_LOOP ( 'NONE', ( #17950, #9923, #1893, #5498 ) ) ;
#12205 = LINE ( 'NONE', #1023, #11615 ) ;
#12206 = CARTESIAN_POINT ( 'NONE',  ( 25.37918902992234393, 10.00000000000000000, 1.000000000000000000 ) ) ;
#12207 = EDGE_LOOP ( 'NONE', ( #19528, #17848, #12323, #1357 ) ) ;
#12208 = CARTESIAN_POINT ( 'NONE',  ( 1.700193846275138032, -9.865151716929458914, 2.372704024825938340 ) ) ;
#12209 = ORIENTED_EDGE ( 'NONE', *, *, #2204, .F. ) ;
#12210 = ADVANCED_FACE ( 'NONE', ( #12601 ), #19314, .T. ) ;
#12211 = EDGE_CURVE ( 'NONE', #8663, #3716, #9372, .T. ) ;
#12212 = VECTOR ( 'NONE', #19955, 1000.000000000000000 ) ;
#12213 = ORIENTED_EDGE ( 'NONE', *, *, #3614, .F. ) ;
#12214 = DIRECTION ( 'NONE',  ( 0.000000000000000000, 1.000000000000000000, 0.000000000000000000 ) ) ;
#12215 = CARTESIAN_POINT ( 'NONE',  ( 7.499999999999999112, -25.49999999999999645, 4.000000000000000000 ) ) ;
#12216 = CARTESIAN_POINT ( 'NONE',  ( -1.619022621591186928, -9.864917468222230923, 1.622643865078341907 ) ) ;
#12217 = FACE_OUTER_BOUND ( 'NONE', #12718, .T. ) ;
#12218 = CARTESIAN_POINT ( 'NONE',  ( 0.000000000000000000, 0.000000000000000000, 4.000000000000000000 ) ) ;
#12219 = CARTESIAN_POINT ( 'NONE',  ( -14.49999999999998579, -18.49999999999999645, 1.000000000000000000 ) ) ;
#12220 = CARTESIAN_POINT ( 'NONE',  ( 11.12844141768317741, -19.49999999999998934, 3.550687472877664952 ) ) ;
#12221 = CARTESIAN_POINT ( 'NONE',  ( -12.74043380832193684, -14.42059267975384529, 5.611358176248560703 ) ) ;
#12222 = EDGE_CURVE ( 'NONE', #10614, #8228, #3036, .T. ) ;
#12223 = CARTESIAN_POINT ( 'NONE',  ( -11.22219141768317741, -20.27099543870833998, 4.275561207030583510 ) ) ;
#12224 = EDGE_LOOP ( 'NONE', ( #5881, #11467, #9278, #14575 ) ) ;
#12225 = CARTESIAN_POINT ( 'NONE',  ( 11.68405858231679417, -20.79840458871652942, 2.226721677130544030 ) ) ;
#12226 = DIRECTION ( 'NONE',  ( 0.000000000000000000, 0.000000000000000000, 1.000000000000000000 ) ) ;
#12227 = CARTESIAN_POINT ( 'NONE',  ( -13.39169349927020569, -20.15697828685464188, 6.009339318877812808 ) ) ;
#12228 = CARTESIAN_POINT ( 'NONE',  ( 10.84030858231679240, -22.67418626127525982, 5.270995438708342640 ) ) ;
#12229 = CARTESIAN_POINT ( 'NONE',  ( -20.92243175760212637, 4.999999999999999112, 0.000000000000000000 ) ) ;
#12230 = VERTEX_POINT ( 'NONE', #9677 ) ;
#12231 = ORIENTED_EDGE ( 'NONE', *, *, #2957, .F. ) ;
#12232 = CARTESIAN_POINT ( 'NONE',  ( 13.37499964066394043, -21.00001814646822496, 4.442866346476199269 ) ) ;
#12233 = DIRECTION ( 'NONE',  ( 1.000000000000000000, 0.000000000000000000, 0.000000000000000000 ) ) ;
#12234 = ORIENTED_EDGE ( 'NONE', *, *, #19862, .T. ) ;
#12235 = DIRECTION ( 'NONE',  ( 1.000000000000000000, 0.000000000000000000, -0.000000000000000000 ) ) ;
#12236 = VERTEX_POINT ( 'NONE', #7809 ) ;
#12237 = CARTESIAN_POINT ( 'NONE',  ( -8.496558582316794173, -22.05068747287764452, 1.749999999999998446 ) ) ;
#12238 = CARTESIAN_POINT ( 'NONE',  ( 5.683390479346035029, 9.000000000000001776, 1.000000000000000000 ) ) ;
#12239 = CYLINDRICAL_SURFACE ( 'NONE', #2177, 0.3749999999999997224 ) ;
#12240 = CARTESIAN_POINT ( 'NONE',  ( 1.798207051321043304, -8.367281747657623114, 1.623251059268568053 ) ) ;
#12241 = AXIS2_PLACEMENT_3D ( 'NONE', #16255, #9562, #153 ) ;
#12242 = DIRECTION ( 'NONE',  ( 0.000000000000000000, -1.000000000000000000, 0.000000000000000000 ) ) ;
#12243 = CARTESIAN_POINT ( 'NONE',  ( -13.37499999999998224, -19.49999999999998934, 4.291666666666699825 ) ) ;
#12244 = CARTESIAN_POINT ( 'NONE',  ( 13.09030858231679417, -21.32581373872472597, 1.729004561291657582 ) ) ;
#12245 = CARTESIAN_POINT ( 'NONE',  ( -13.37500000000002132, -20.99999999999450395, 3.833333333368183382 ) ) ;
#12246 = ADVANCED_FACE ( 'NONE', ( #11245 ), #20473, .F. ) ;
#12247 = DIRECTION ( 'NONE',  ( 1.000000000000000000, -0.000000000000000000, 0.000000000000000000 ) ) ;
#12248 = CARTESIAN_POINT ( 'NONE',  ( 12.24655858231679240, -21.94931252712234482, 5.250000000000000888 ) ) ;
#12249 = CARTESIAN_POINT ( 'NONE',  ( 5.690941417683176518, -23.27327832286946219, 4.701595411283453707 ) ) ;
#12250 = CARTESIAN_POINT ( 'NONE',  ( -6.246558582316794173, -21.94931252712234482, 5.250000000000000888 ) ) ;
#12251 = VERTEX_POINT ( 'NONE', #10268 ) ;
#12252 = CARTESIAN_POINT ( 'NONE',  ( 13.37499999999998401, -19.49999999999998934, 2.439580858552613751 ) ) ;
#12253 = DIRECTION ( 'NONE',  ( 1.000000000000000000, 0.000000000000000000, 0.000000000000000000 ) ) ;
#12254 = EDGE_LOOP ( 'NONE', ( #7280, #19300, #908, #5446 ) ) ;
#12255 = ORIENTED_EDGE ( 'NONE', *, *, #7708, .T. ) ;
#12256 = DIRECTION ( 'NONE',  ( 0.000000000000000000, -1.000000000000000000, 0.000000000000000000 ) ) ;
#12257 = PRODUCT_DEFINITION ( 'UNKNOWN', '', #17378, #3161 ) ;
#12258 = CARTESIAN_POINT ( 'NONE',  ( -13.09532840572934376, 3.501584489333809724, 5.996774842915142401 ) ) ;
#12259 = FACE_OUTER_BOUND ( 'NONE', #6991, .T. ) ;
#12260 = CARTESIAN_POINT ( 'NONE',  ( -13.38800411018677572, -19.59329243556743805, 5.436267741224407146 ) ) ;
#12261 = DIRECTION ( 'NONE',  ( 0.000000000000000000, -0.000000000000000000, 1.000000000000000000 ) ) ;
#12262 = LINE ( 'NONE', #9137, #9203 ) ;
#12263 = FACE_OUTER_BOUND ( 'NONE', #8585, .T. ) ;
#12264 = CARTESIAN_POINT ( 'NONE',  ( 24.62918902992234038, 0.000000000000000000, 1.000000000000000000 ) ) ;
#12265 = CARTESIAN_POINT ( 'NONE',  ( 4.687312169500630787, -21.51559725698340131, 5.182386163300424009 ) ) ;
#12266 = CARTESIAN_POINT ( 'NONE',  ( -8.309058582316795949, -23.80360840875935935, 1.768074502826626260 ) ) ;
#12267 = CARTESIAN_POINT ( 'NONE',  ( -1.852280067228949445, -9.126254559850970338, 1.625555456689752321 ) ) ;
#12268 = ORIENTED_EDGE ( 'NONE', *, *, #19253, .F. ) ;
#12269 = CARTESIAN_POINT ( 'NONE',  ( -13.37741471237955260, -20.12805702483293757, 4.993653275319895890 ) ) ;
#12270 = CYLINDRICAL_SURFACE ( 'NONE', #16723, 0.2500000000000002220 ) ;
#12271 = EDGE_CURVE ( 'NONE', #4847, #9411, #3577, .T. ) ;
#12273 = CARTESIAN_POINT ( 'NONE',  ( 12.62844141768317741, -19.49999999999998934, 3.550687472877664952 ) ) ;
#12272 = APPLICATION_CONTEXT ( 'automotive_design' ) ;
#12274 = CARTESIAN_POINT ( 'NONE',  ( -9.440941417683177406, -21.25705176302044208, 2.828734674606458555 ) ) ;
#12275 = EDGE_LOOP ( 'NONE', ( #16295, #4032, #1482, #11408 ) ) ;
#12276 = CARTESIAN_POINT ( 'NONE',  ( 13.86106797245302147, 4.296432608878145487, 5.947261916831099171 ) ) ;
#12277 = CARTESIAN_POINT ( 'NONE',  ( 12.62515553039088090, -20.24214571525854467, 4.629702272822510345 ) ) ;
#12278 = ORIENTED_EDGE ( 'NONE', *, *, #17722, .T. ) ;
#12279 = ORIENTED_EDGE ( 'NONE', *, *, #7427, .T. ) ;
#12280 = CARTESIAN_POINT ( 'NONE',  ( 8.876396343307449754, 10.00000000000000000, 0.000000000000000000 ) ) ;
#12281 = EDGE_LOOP ( 'NONE', ( #20617, #4613, #13557, #7022 ) ) ;
#12282 = CARTESIAN_POINT ( 'NONE',  ( -13.87470602645761808, 4.985154336109792972, 4.000000000000000000 ) ) ;
#12283 = ADVANCED_FACE ( 'NONE', ( #16637 ), #11429, .T. ) ;
#12284 = ADVANCED_FACE ( 'NONE', ( #18226 ), #17814, .T. ) ;
#12285 = CARTESIAN_POINT ( 'NONE',  ( -5.933390479346035029, 9.000000000000001776, 1.000000000000000000 ) ) ;
#12286 = ORIENTED_EDGE ( 'NONE', *, *, #10245, .F. ) ;
#12287 = DIRECTION ( 'NONE',  ( -0.000000000000000000, 0.000000000000000000, -1.000000000000000000 ) ) ;
#12288 = LINE ( 'NONE', #2674, #10680 ) ;
#12289 = DIRECTION ( 'NONE',  ( 1.000000000000000000, 0.000000000000000000, 0.000000000000000000 ) ) ;
#12290 = CARTESIAN_POINT ( 'NONE',  ( 2.708677329869237482, -9.785633270066144362, 1.794897081886200230 ) ) ;
#12291 = CARTESIAN_POINT ( 'NONE',  ( -9.999999999999998224, -30.00000000000000355, 1.000000000000000000 ) ) ;
#12292 = CARTESIAN_POINT ( 'NONE',  ( 13.12526104302547836, 5.013182672784613381, 5.066812735559260261 ) ) ;
#12293 = CARTESIAN_POINT ( 'NONE',  ( 0.000000000000000000, 11.64110105645932691, 10.00000000000000000 ) ) ;
#12294 = CARTESIAN_POINT ( 'NONE',  ( 5.000000000000000000, 0.000000000000000000, 0.000000000000000000 ) ) ;
#12295 = LINE ( 'NONE', #2891, #10039 ) ;
#12296 = CARTESIAN_POINT ( 'NONE',  ( 8.878441417683177406, -22.99999999999999645, 3.449312527122335048 ) ) ;
#12297 = CARTESIAN_POINT ( 'NONE',  ( -13.11145189917479392, 4.315820908324673688, 5.961432613039677086 ) ) ;
#12298 = CARTESIAN_POINT ( 'NONE',  ( -7.371558582316795949, -20.99999999999999645, 3.449312527122348371 ) ) ;
#12299 = EDGE_CURVE ( 'NONE', #9021, #4521, #759, .T. ) ;
#12300 = CARTESIAN_POINT ( 'NONE',  ( -11.40969141768317918, -21.01515356694492098, 6.020995438708349745 ) ) ;
#12301 = AXIS2_PLACEMENT_3D ( 'NONE', #9265, #7702, #13761 ) ;
#12302 = ORIENTED_EDGE ( 'NONE', *, *, #970, .T. ) ;
#12303 = CARTESIAN_POINT ( 'NONE',  ( 12.62966097655984754, -19.26462068372267566, 4.756751955311774083 ) ) ;
#12304 = CARTESIAN_POINT ( 'NONE',  ( -13.11740841389447709, 4.616624901677048420, 5.813473370769506765 ) ) ;
#12305 = ORIENTED_EDGE ( 'NONE', *, *, #6337, .T. ) ;
#12306 = DIRECTION ( 'NONE',  ( 1.000000000000000000, 0.000000000000000000, 0.000000000000000000 ) ) ;
#12307 = ORIENTED_EDGE ( 'NONE', *, *, #16479, .F. ) ;
#12308 = CARTESIAN_POINT ( 'NONE',  ( 1.791727654783324741, -9.894249715907907472, 2.380176972254574697 ) ) ;
#12309 = EDGE_CURVE ( 'NONE', #16469, #13516, #10583, .T. ) ;
#12310 = EDGE_CURVE ( 'NONE', #14610, #8663, #5038, .T. ) ;
#12311 = VECTOR ( 'NONE', #18141, 1000.000000000000000 ) ;
#12312 = VERTEX_POINT ( 'NONE', #18329 ) ;
#12313 = DIRECTION ( 'NONE',  ( 0.000000000000000000, 0.000000000000000000, -1.000000000000000000 ) ) ;
#12314 = LINE ( 'NONE', #18603, #10305 ) ;
#12315 = CARTESIAN_POINT ( 'NONE',  ( -1.744064896197293324, -9.868721669903177229, 1.623620860066563365 ) ) ;
#12316 = DIRECTION ( 'NONE',  ( 4.625929269271477434E-15, 1.000000000000000000, 0.000000000000000000 ) ) ;
#12317 = CARTESIAN_POINT ( 'NONE',  ( 20.50349085826861995, 16.00000000000000000, 1.000000000000000000 ) ) ;
#12318 = CARTESIAN_POINT ( 'NONE',  ( 1.937849085826861328, 10.00000000000000000, 0.000000000000000000 ) ) ;
#12319 = CARTESIAN_POINT ( 'NONE',  ( 5.409691417683178294, -21.01515356694492098, 6.020995438708349745 ) ) ;
#12320 = CARTESIAN_POINT ( 'NONE',  ( -12.64691428603184242, -19.14332855539073464, 5.509795676248469221 ) ) ;
#12321 = CARTESIAN_POINT ( 'NONE',  ( -11.40969141768318096, -21.32581373872474373, 5.270995438708348857 ) ) ;
#12322 = ADVANCED_FACE ( 'NONE', ( #12147 ), #4100, .F. ) ;
#12323 = ORIENTED_EDGE ( 'NONE', *, *, #5507, .T. ) ;
#12324 = EDGE_CURVE ( 'NONE', #2944, #4223, #10483, .T. ) ;
#12325 = CARTESIAN_POINT ( 'NONE',  ( 12.99655858231679417, -22.05068747287764452, 1.749999999999998446 ) ) ;
#12326 = DIRECTION ( 'NONE',  ( 0.000000000000000000, -1.000000000000000000, 0.000000000000000000 ) ) ;
#12327 = CARTESIAN_POINT ( 'NONE',  ( -13.37499999999998224, -20.99999999999998934, 4.291666666666699825 ) ) ;
#12328 = VECTOR ( 'NONE', #5580, 1000.000000000000000 ) ;
#12329 = CARTESIAN_POINT ( 'NONE',  ( 6.152808582316795949, -21.53509896474924901, 4.479004561291659137 ) ) ;
#12330 = CARTESIAN_POINT ( 'NONE',  ( 11.49178095869207006, 4.999999999999999112, 1.000000000000000000 ) ) ;
#12331 = AXIS2_PLACEMENT_3D ( 'NONE', #6684, #11181, #17657 ) ;
#12332 = EDGE_LOOP ( 'NONE', ( #1177, #11088, #6810, #13530, #217, #16049, #15752 ) ) ;
#12333 = ORIENTED_EDGE ( 'NONE', *, *, #81, .F. ) ;
#12334 = CARTESIAN_POINT ( 'NONE',  ( 13.38172782443493602, -20.66024486603417643, 5.557997437521964734 ) ) ;
#12335 = PRODUCT_DEFINITION_SHAPE ( 'NONE', 'NONE',  #20723 ) ;
#12336 = LINE ( 'NONE', #18421, #3249 ) ;
#12337 = SURFACE_STYLE_FILL_AREA ( #1260 ) ;
#12338 = VERTEX_POINT ( 'NONE', #17165 ) ;
#12339 = LINE ( 'NONE', #10572, #770 ) ;
#12340 = ORIENTED_EDGE ( 'NONE', *, *, #5779, .F. ) ;
#12341 = ADVANCED_FACE ( 'NONE', ( #2740 ), #10377, .T. ) ;
#12342 = CARTESIAN_POINT ( 'NONE',  ( -12.52780858231679595, -23.72900456129165647, 4.275561207030568411 ) ) ;
#12343 = FACE_OUTER_BOUND ( 'NONE', #15466, .T. ) ;
#12344 = DIRECTION ( 'NONE',  ( 0.000000000000000000, 0.000000000000000000, 1.000000000000000000 ) ) ;
#12345 = CARTESIAN_POINT ( 'NONE',  ( 1.852280067228949445, -9.126254559850970338, 1.625555456689752321 ) ) ;
#12346 = AXIS2_PLACEMENT_3D ( 'NONE', #16646, #5571, #2324 ) ;
#12347 = DIRECTION ( 'NONE',  ( 1.000000000000000000, 0.000000000000000000, 0.000000000000000000 ) ) ;
#12348 = CARTESIAN_POINT ( 'NONE',  ( -13.37908441539295801, -19.29373702265862889, 4.740102594697787275 ) ) ;
#12349 = CARTESIAN_POINT ( 'NONE',  ( 13.37155858231679417, -20.24999999999999289, 3.449312527122348371 ) ) ;
#12350 = CARTESIAN_POINT ( 'NONE',  ( -13.37526900345969771, -20.98641532528209908, 4.724331462949078464 ) ) ;
#12351 = VECTOR ( 'NONE', #14121, 1000.000000000000000 ) ;
#12352 = ADVANCED_FACE ( 'NONE', ( #12354 ), #2520, .T. ) ;
#12353 = ADVANCED_FACE ( 'NONE', ( #7144 ), #15280, .T. ) ;
#12354 = FACE_OUTER_BOUND ( 'NONE', #15425, .T. ) ;
#12355 = CARTESIAN_POINT ( 'NONE',  ( 6.340308582316796837, -22.36352608949544418, 4.520995438708343528 ) ) ;
#12356 = CARTESIAN_POINT ( 'NONE',  ( 9.722191417683177406, -21.02099543870834353, 3.964901035250761208 ) ) ;
#12357 = CARTESIAN_POINT ( 'NONE',  ( -11.31594141768317741, -20.79840458871654363, 4.773278322869464851 ) ) ;
#12358 = VERTEX_POINT ( 'NONE', #9017 ) ;
#12359 = CARTESIAN_POINT ( 'NONE',  ( 13.37500751150753864, -19.49962066887028556, 4.515663405036051792 ) ) ;
#12360 = VECTOR ( 'NONE', #7780, 1000.000000000000000 ) ;
#12361 = CARTESIAN_POINT ( 'NONE',  ( -0.1250000000000035805, 0.000000000000000000, 1.000000000000000000 ) ) ;
#12362 = ORIENTED_EDGE ( 'NONE', *, *, #1962, .F. ) ;
#12363 = ORIENTED_EDGE ( 'NONE', *, *, #17788, .F. ) ;
#12364 = DIRECTION ( 'NONE',  ( 1.000000000000000000, 6.938893903907232322E-16, -0.000000000000000000 ) ) ;
#12365 = EDGE_CURVE ( 'NONE', #15652, #5903, #11935, .T. ) ;
#12366 = AXIS2_PLACEMENT_3D ( 'NONE', #4147, #6032, #18585 ) ;
#12367 = CARTESIAN_POINT ( 'NONE',  ( -12.62672070884157804, -20.24999999999991473, 3.550922209436377042 ) ) ;
#12368 = CARTESIAN_POINT ( 'NONE',  ( -1.957016269584227031, -9.152392576945766578, 2.382268221639079364 ) ) ;
#12369 = CARTESIAN_POINT ( 'NONE',  ( -13.87470602645761986, 4.985154336109792972, 4.916666666666650087 ) ) ;
#12370 = CARTESIAN_POINT ( 'NONE',  ( 0.000000000000000000, 11.64110105645932691, 10.00000000000000000 ) ) ;
#12371 = CARTESIAN_POINT ( 'NONE',  ( -12.62499999998404121, -20.24999999996810729, 2.793053905886972998 ) ) ;
#12372 = CARTESIAN_POINT ( 'NONE',  ( 0.000000000000000000, 4.999999999999999112, 1.000000000000000000 ) ) ;
#12373 = LINE ( 'NONE', #4434, #16079 ) ;
#12374 = PRODUCT_DEFINITION_FORMATION_WITH_SPECIFIED_SOURCE ( 'ANY', '', #2828, .NOT_KNOWN. ) ;
#12375 = PLANE ( 'NONE',  #3627 ) ;
#12376 = CARTESIAN_POINT ( 'NONE',  ( -13.09030858231679417, -21.01515356694490322, 0.9790045612916562501 ) ) ;
#12377 = CARTESIAN_POINT ( 'NONE',  ( -2.282685604506861754, -11.80366834561962364, 2.120553820834011116 ) ) ;
#12378 = ORIENTED_EDGE ( 'NONE', *, *, #9847, .T. ) ;
#12379 = CARTESIAN_POINT ( 'NONE',  ( -13.37500000000002132, -20.24999999999450040, 3.833333333368183382 ) ) ;
#12380 = AXIS2_PLACEMENT_3D ( 'NONE', #10412, #7174, #2350 ) ;
#12381 = CARTESIAN_POINT ( 'NONE',  ( 11.00000000000000000, -23.83493649053891517, 5.249999999999999112 ) ) ;
#12382 = VECTOR ( 'NONE', #17497, 1000.000000000000000 ) ;
#12383 = CARTESIAN_POINT ( 'NONE',  ( 6.152808582316795949, -20.91377862118960351, 5.979004561291660913 ) ) ;
#12384 = CARTESIAN_POINT ( 'NONE',  ( -5.972191417683178294, -22.97900456129165292, 3.035098964749240125 ) ) ;
#12385 = VERTEX_POINT ( 'NONE', #957 ) ;
#12386 = CARTESIAN_POINT ( 'NONE',  ( 13.37499999999998401, -20.99999999999999645, 3.146526952850934755 ) ) ;
#12387 = ORIENTED_EDGE ( 'NONE', *, *, #3665, .T. ) ;
#12388 = ORIENTED_EDGE ( 'NONE', *, *, #7331, .F. ) ;
#12389 = PLANE ( 'NONE',  #18463 ) ;
#12390 = VERTEX_POINT ( 'NONE', #18748 ) ;
#12391 = CARTESIAN_POINT ( 'NONE',  ( -13.66279757975024722, -5.716222222589476765, 5.784013032957989964 ) ) ;
#12392 = PLANE ( 'NONE',  #3785 ) ;
#12393 = ORIENTED_EDGE ( 'NONE', *, *, #7678, .T. ) ;
#12394 = DIRECTION ( 'NONE',  ( 1.000000000000000000, 0.000000000000000000, -0.000000000000000000 ) ) ;
#12395 = CARTESIAN_POINT ( 'NONE',  ( 2.817596665886821672, -11.50588678273290988, 2.986692549455723267 ) ) ;
#12396 = VECTOR ( 'NONE', #14347, 1000.000000000000000 ) ;
#12397 = EDGE_CURVE ( 'NONE', #378, #17017, #9217, .T. ) ;
#12398 = VECTOR ( 'NONE', #228, 1000.000000000000000 ) ;
#12399 = CARTESIAN_POINT ( 'NONE',  ( 15.06494360078803041, 16.00000000000000000, 1.000000000000000000 ) ) ;
#12400 = CARTESIAN_POINT ( 'NONE',  ( 0.5631383031621635116, -8.364917468222230923, 1.622643865078341907 ) ) ;
#12401 = CARTESIAN_POINT ( 'NONE',  ( 0.000000000000000000, 0.000000000000000000, 0.5000000000000000000 ) ) ;
#12402 = DIRECTION ( 'NONE',  ( 0.000000000000000000, -0.000000000000000000, 1.000000000000000000 ) ) ;
#12403 = CARTESIAN_POINT ( 'NONE',  ( -27.00000000000000000, 3.000000000000000000, 1.000000000000000000 ) ) ;
#12404 = DIRECTION ( 'NONE',  ( 0.000000000000000000, 0.000000000000000000, -1.000000000000000000 ) ) ;
#12405 = DIRECTION ( 'NONE',  ( 1.000000000000000000, 1.156482317317871133E-15, -0.000000000000000000 ) ) ;
#12406 = CARTESIAN_POINT ( 'NONE',  ( 12.99655858231679595, -22.05068747287764452, 2.499999999999999112 ) ) ;
#12407 = CARTESIAN_POINT ( 'NONE',  ( -13.12529397354238192, 5.014845663890295846, 3.666666666666500873 ) ) ;
#12408 = CARTESIAN_POINT ( 'NONE',  ( -7.746558582316795949, -21.94931252712234127, 4.499999999999999112 ) ) ;
#12409 = CARTESIAN_POINT ( 'NONE',  ( -4.847191417683177406, -20.91377862118959285, 1.020995438708345082 ) ) ;
#12410 = ORIENTED_EDGE ( 'NONE', *, *, #5673, .T. ) ;
#12411 = CARTESIAN_POINT ( 'NONE',  ( 13.37514942709654164, -19.49245393162283690, 4.562067678168288509 ) ) ;
#12412 = CARTESIAN_POINT ( 'NONE',  ( -17.05017143803810242, 4.999999999999999112, 1.000000000000000000 ) ) ;
#12413 = ORIENTED_EDGE ( 'NONE', *, *, #3472, .T. ) ;
#12414 = VECTOR ( 'NONE', #12839, 1000.000000000000000 ) ;
#12415 = DIRECTION ( 'NONE',  ( -1.000000000000000000, 0.000000000000000000, 0.000000000000000000 ) ) ;
#12416 = ORIENTED_EDGE ( 'NONE', *, *, #6815, .T. ) ;
#12417 = CARTESIAN_POINT ( 'NONE',  ( 1.862510824048270619, -9.990417728039201251, 2.404874838918925395 ) ) ;
#12418 = ORIENTED_EDGE ( 'NONE', *, *, #13111, .F. ) ;
#12419 = CARTESIAN_POINT ( 'NONE',  ( 0.000000000000000000, 4.999999999999999112, 1.000000000000000000 ) ) ;
#12420 = CARTESIAN_POINT ( 'NONE',  ( 0.000000000000000000, 4.999999999999999112, 1.000000000000000000 ) ) ;
#12421 = ADVANCED_FACE ( 'NONE', ( #13603 ), #4412, .T. ) ;
#12422 = CARTESIAN_POINT ( 'NONE',  ( -1.982945319006538032, -10.83166796549307520, 2.620924705558935308 ) ) ;
#12423 = DIRECTION ( 'NONE',  ( -0.000000000000000000, 1.000000000000000000, -0.000000000000000000 ) ) ;
#12424 = CARTESIAN_POINT ( 'NONE',  ( 13.92791111847407848, 4.999999999999999112, 1.000000000000000000 ) ) ;
#12425 = AXIS2_PLACEMENT_3D ( 'NONE', #160, #3520, #17437 ) ;
#12426 = LINE ( 'NONE', #4683, #2612 ) ;
#12427 = ADVANCED_FACE ( 'NONE', ( #5777 ), #7452, .T. ) ;
#12428 = EDGE_CURVE ( 'NONE', #1844, #1315, #20008, .T. ) ;
#12429 = CARTESIAN_POINT ( 'NONE',  ( 4.003441417683175629, -22.05068747287766229, 6.000000000000001776 ) ) ;
#12430 = CARTESIAN_POINT ( 'NONE',  ( -9.440941417683177406, -20.72672167713052715, 2.298404588716546293 ) ) ;
#12431 = ORIENTED_EDGE ( 'NONE', *, *, #12582, .F. ) ;
#12432 = CARTESIAN_POINT ( 'NONE',  ( 8.684058582316794173, -20.79840458871652942, 2.226721677130544030 ) ) ;
#12433 = CARTESIAN_POINT ( 'NONE',  ( -12.00000000000000000, -25.49999999999998934, 1.000000000000000000 ) ) ;
#12434 = CARTESIAN_POINT ( 'NONE',  ( -12.62672826945118665, -20.91272239271162903, 5.058631648758789900 ) ) ;
#12435 = VERTEX_POINT ( 'NONE', #1171 ) ;
#12436 = CARTESIAN_POINT ( 'NONE',  ( -7.499999999999999112, -18.49999999999999645, 4.000000000000000000 ) ) ;
#12437 = PLANE ( 'NONE',  #16003 ) ;
#12438 = ORIENTED_EDGE ( 'NONE', *, *, #14321, .T. ) ;
#12439 = VERTEX_POINT ( 'NONE', #13913 ) ;
#12440 = CARTESIAN_POINT ( 'NONE',  ( 13.77324158252158171, -0.8888000826463379189, 6.637859435864801760 ) ) ;
#12441 = DIRECTION ( 'NONE',  ( -1.000000000000000000, -2.312964634635730039E-15, 0.000000000000000000 ) ) ;
#12442 = SURFACE_STYLE_USAGE ( .BOTH. , #20412 ) ;
#12443 = VERTEX_POINT ( 'NONE', #18436 ) ;
#12444 = AXIS2_PLACEMENT_3D ( 'NONE', #2027, #3804, #2227 ) ;
#12445 = DIRECTION ( 'NONE',  ( -1.000000000000000000, -0.000000000000000000, -0.000000000000000000 ) ) ;
#12446 = ORIENTED_EDGE ( 'NONE', *, *, #16038, .T. ) ;
#12447 = CARTESIAN_POINT ( 'NONE',  ( -12.71530858231679240, -23.77099543870833998, 2.825813738724734847 ) ) ;
#12448 = PLANE ( 'NONE',  #11923 ) ;
#12449 = EDGE_CURVE ( 'NONE', #5966, #8747, #10690, .T. ) ;
#12450 = FACE_OUTER_BOUND ( 'NONE', #16455, .T. ) ;
#12451 = CARTESIAN_POINT ( 'NONE',  ( 2.708677329869237482, -9.785633270066144362, 1.794897081886200230 ) ) ;
#12452 = DIRECTION ( 'NONE',  ( -0.000000000000000000, -0.000000000000000000, -1.000000000000000000 ) ) ;
#12453 = CARTESIAN_POINT ( 'NONE',  ( -13.07840392524817474, 3.396898225032857432, 5.244490940007585422 ) ) ;
#12454 = CARTESIAN_POINT ( 'NONE',  ( 9.902808582316794173, -22.77556120703056308, 1.770995438708339975 ) ) ;
#12455 = CARTESIAN_POINT ( 'NONE',  ( -12.65346245025441263, -19.56264626215117275, 6.228892365149262922 ) ) ;
#12456 = CIRCLE ( 'NONE', #10464, 0.2500000000000002220 ) ;
#12457 = CARTESIAN_POINT ( 'NONE',  ( -23.35856191738413656, 0.000000000000000000, 0.000000000000000000 ) ) ;
#12458 = CARTESIAN_POINT ( 'NONE',  ( 12.62155858231679417, -23.74999999999999645, 3.550687472877651629 ) ) ;
#12459 = EDGE_CURVE ( 'NONE', #9247, #19171, #20315, .T. ) ;
#12460 = CARTESIAN_POINT ( 'NONE',  ( 9.253441417683177406, -21.94931252712233061, 2.499999999999999112 ) ) ;
#12461 = CARTESIAN_POINT ( 'NONE',  ( -4.746558582316793284, -21.94931252712234482, 5.250000000000000888 ) ) ;
#12462 = ORIENTED_EDGE ( 'NONE', *, *, #7451, .F. ) ;
#12463 = CARTESIAN_POINT ( 'NONE',  ( 13.38449802415168932, -19.02034978033825396, 4.747874963382372471 ) ) ;
#12464 = CARTESIAN_POINT ( 'NONE',  ( -2.739050625766161762, -9.875938058683834342, 1.818089155622620412 ) ) ;
#12465 = ORIENTED_EDGE ( 'NONE', *, *, #6734, .T. ) ;
#12466 = ORIENTED_EDGE ( 'NONE', *, *, #17229, .F. ) ;
#12467 = CARTESIAN_POINT ( 'NONE',  ( 5.000000000000000000, -12.50000000000000000, 1.000000000000000000 ) ) ;
#12468 = CARTESIAN_POINT ( 'NONE',  ( -13.10192273101908000, 3.834597916462216816, 6.003936301248457674 ) ) ;
#12469 = EDGE_CURVE ( 'NONE', #12236, #17290, #16004, .T. ) ;
#12470 = EDGE_CURVE ( 'NONE', #17893, #9631, #7949, .T. ) ;
#12471 = CARTESIAN_POINT ( 'NONE',  ( -4.181771508648414404, -14.78356139460145968, 3.271079850667843125 ) ) ;
#12472 = CARTESIAN_POINT ( 'NONE',  ( -13.85788212999909419, 4.135547564954428879, 5.982801014393342776 ) ) ;
#12473 = EDGE_CURVE ( 'NONE', #18369, #8256, #4687, .T. ) ;
#12474 = CARTESIAN_POINT ( 'NONE',  ( 27.52582389412042474, 4.853545418763153485, 1.000000000000000000 ) ) ;
#12475 = LINE ( 'NONE', #2858, #7537 ) ;
#12476 = CARTESIAN_POINT ( 'NONE',  ( -23.35856191738413656, 9.000000000000001776, 1.000000000000000000 ) ) ;
#12477 = CARTESIAN_POINT ( 'NONE',  ( 23.60856191738414012, 9.000000000000001776, 1.000000000000000000 ) ) ;
#12478 = AXIS2_PLACEMENT_3D ( 'NONE', #13276, #17896, #3775 ) ;
#12479 = CARTESIAN_POINT ( 'NONE',  ( -10.09030858231679595, -21.01515356694490322, 0.9790045612916562501 ) ) ;
#12480 = CARTESIAN_POINT ( 'NONE',  ( -1.865667289525601680, -9.999006358835732300, 2.407080570882605297 ) ) ;
#12481 = EDGE_LOOP ( 'NONE', ( #10609, #13802, #482, #7271 ) ) ;
#12482 = CARTESIAN_POINT ( 'NONE',  ( -13.84501469867711698, 4.235742283194553259, 4.666666666666618113 ) ) ;
#12483 = CARTESIAN_POINT ( 'NONE',  ( 17.80017143803810242, 9.000000000000001776, 0.000000000000000000 ) ) ;
#12484 = EDGE_CURVE ( 'NONE', #15255, #8718, #6184, .T. ) ;
#12485 = CARTESIAN_POINT ( 'NONE',  ( 6.527808582316795949, -24.47900456129166358, 4.586221378810390270 ) ) ;
#12486 = CARTESIAN_POINT ( 'NONE',  ( -6.722191417683176518, -21.02099543870834353, 3.964901035250761208 ) ) ;
#12487 = VERTEX_POINT ( 'NONE', #8069 ) ;
#12488 = CARTESIAN_POINT ( 'NONE',  ( 13.41175265982446696, -19.14399067886409256, 6.245281310864100988 ) ) ;
#12489 = CARTESIAN_POINT ( 'NONE',  ( 12.62500016093973620, -20.24999187254239175, 4.532396751752561848 ) ) ;
#12490 = EDGE_LOOP ( 'NONE', ( #9815, #7481, #3116, #7582 ) ) ;
#12491 = VERTEX_POINT ( 'NONE', #11294 ) ;
#12492 = LINE ( 'NONE', #6123, #8818 ) ;
#12493 = ORIENTED_EDGE ( 'NONE', *, *, #2951, .T. ) ;
#12494 = CARTESIAN_POINT ( 'NONE',  ( -13.87444723674697755, 4.972085455720938185, 5.163895512850782410 ) ) ;
#12495 = CARTESIAN_POINT ( 'NONE',  ( 0.9854920305337621089, -9.114917468222230923, 2.372643865078341019 ) ) ;
#12496 = CARTESIAN_POINT ( 'NONE',  ( 0.000000000000000000, 10.00000000000000000, 1.000000000000000000 ) ) ;
#12497 = CARTESIAN_POINT ( 'NONE',  ( 13.50000000000001243, -19.49999999999999645, 4.000000000000000000 ) ) ;
#12498 = CARTESIAN_POINT ( 'NONE',  ( 2.623717082130370137, -10.12934627674766830, 2.633169448359191644 ) ) ;
#12499 = DIRECTION ( 'NONE',  ( 0.000000000000000000, -0.000000000000000000, 1.000000000000000000 ) ) ;
#12500 = CARTESIAN_POINT ( 'NONE',  ( 1.754777266914451461, -9.116337928146160507, 1.623008667563337726 ) ) ;
#12501 = FACE_OUTER_BOUND ( 'NONE', #19270, .T. ) ;
#12502 = CARTESIAN_POINT ( 'NONE',  ( 13.12503131243110843, 5.001581277770153378, 5.166347330538456184 ) ) ;
#12503 = CARTESIAN_POINT ( 'NONE',  ( -15.00000000000000000, 3.000000000000000000, 2.000000000000000000 ) ) ;
#12504 = LINE ( 'NONE', #7401, #7030 ) ;
#12505 = FACE_OUTER_BOUND ( 'NONE', #3110, .T. ) ;
#12506 = CARTESIAN_POINT ( 'NONE',  ( 6.534691417683177406, -20.97900456129164581, 3.136473910504570917 ) ) ;
#12507 = CARTESIAN_POINT ( 'NONE',  ( -13.10431844137356627, 3.955581289335645234, 6.006545679920360925 ) ) ;
#12508 = CARTESIAN_POINT ( 'NONE',  ( -10.55905858231679595, -21.25705176302045274, 4.171265325393551215 ) ) ;
#12509 = EDGE_CURVE ( 'NONE', #10573, #19423, #4820, .T. ) ;
#12510 = CARTESIAN_POINT ( 'NONE',  ( -4.190941417683176518, -23.80360840875937001, 5.231925497173365081 ) ) ;
#12511 = ORIENTED_EDGE ( 'NONE', *, *, #17922, .T. ) ;
#12512 = CARTESIAN_POINT ( 'NONE',  ( 13.09559422631463654, 4.265008428887424152, 5.017082219073495608 ) ) ;
#12513 = DIRECTION ( 'NONE',  ( 0.000000000000000000, -1.000000000000000000, 0.000000000000000000 ) ) ;
#12514 = VERTEX_POINT ( 'NONE', #8 ) ;
#12515 = DIRECTION ( 'NONE',  ( 0.000000000000000000, 0.000000000000000000, 1.000000000000000000 ) ) ;
#12516 = ORIENTED_EDGE ( 'NONE', *, *, #15509, .F. ) ;
#12517 = CARTESIAN_POINT ( 'NONE',  ( 1.668644041176298387, -9.864915931696323526, 2.372643470467795890 ) ) ;
#12518 = VECTOR ( 'NONE', #20574, 1000.000000000000000 ) ;
#12519 = EDGE_LOOP ( 'NONE', ( #6162, #7558, #13517, #19245, #916 ) ) ;
#12520 = CARTESIAN_POINT ( 'NONE',  ( -28.94203811574919882, 16.00000000000000000, 1.000000000000000000 ) ) ;
#12521 = CARTESIAN_POINT ( 'NONE',  ( -15.61404127825609223, 0.000000000000000000, 1.000000000000000000 ) ) ;
#12522 = CIRCLE ( 'NONE', #3187, 2.500000000000000444 ) ;
#12523 = CARTESIAN_POINT ( 'NONE',  ( -0.5631383031621635116, -9.114917468222230923, 1.622643865078341463 ) ) ;
#12524 = DIRECTION ( 'NONE',  ( 0.000000000000000000, -1.000000000000000000, 1.304178812473495102E-15 ) ) ;
#12525 = CARTESIAN_POINT ( 'NONE',  ( 19.19064177244175440, 0.000000000000000000, 0.000000000000000000 ) ) ;
#12526 = CARTESIAN_POINT ( 'NONE',  ( 8.972191417683177406, -24.47900456129165292, 2.413778621189595963 ) ) ;
#12527 = CARTESIAN_POINT ( 'NONE',  ( 13.50000000000000178, 5.000000000000047962, 2.000000000000000000 ) ) ;
#12528 = CARTESIAN_POINT ( 'NONE',  ( -9.722191417683177406, -20.27099543870833998, 4.275561207030583510 ) ) ;
#12529 = ORIENTED_EDGE ( 'NONE', *, *, #13519, .F. ) ;
#12530 = CARTESIAN_POINT ( 'NONE',  ( 13.18405858231679595, -20.26807450282662160, 1.696391591240633101 ) ) ;
#12531 = CARTESIAN_POINT ( 'NONE',  ( -11.74178095869206828, 4.999999999999999112, 1.000000000000000000 ) ) ;
#12532 = CARTESIAN_POINT ( 'NONE',  ( -12.92761177809936513, -5.718105205959081339, 6.548537912490751900 ) ) ;
#12533 = EDGE_CURVE ( 'NONE', #4449, #15703, #7651, .T. ) ;
#12534 = CARTESIAN_POINT ( 'NONE',  ( 4.934058582316793284, -23.20159541128345992, 4.773278322869455970 ) ) ;
#12535 = DIRECTION ( 'NONE',  ( -0.000000000000000000, -0.000000000000000000, -1.000000000000000000 ) ) ;
#12536 = ORIENTED_EDGE ( 'NONE', *, *, #10784, .T. ) ;
#12537 = CARTESIAN_POINT ( 'NONE',  ( -13.67791111847408025, 0.000000000000000000, 1.000000000000000000 ) ) ;
#12538 =( NAMED_UNIT ( * ) PLANE_ANGLE_UNIT ( ) SI_UNIT ( $, .RADIAN. ) );
#12539 = EDGE_LOOP ( 'NONE', ( #4445, #10831, #12302, #9843 ) ) ;
#12540 = LINE ( 'NONE', #12749, #8137 ) ;
#12541 = ADVANCED_FACE ( 'NONE', ( #17682 ), #6396, .T. ) ;
#12542 = EDGE_LOOP ( 'NONE', ( #2099, #11392, #8873, #12410 ) ) ;
#12543 = CARTESIAN_POINT ( 'NONE',  ( -13.37155858231679417, -20.24999999999999289, 3.449312527122348371 ) ) ;
#12544 = DIRECTION ( 'NONE',  ( 1.000000000000000000, 0.000000000000000000, 0.000000000000000000 ) ) ;
#12545 = PLANE ( 'NONE',  #2843 ) ;
#12546 = CARTESIAN_POINT ( 'NONE',  ( 2.916276642307554123, -11.05036367517186058, 2.119705115445599475 ) ) ;
#12547 = LINE ( 'NONE', #17362, #15696 ) ;
#12548 = CARTESIAN_POINT ( 'NONE',  ( -13.37732542738919328, -19.38256591684242025, 4.710253041318374301 ) ) ;
#12549 = CARTESIAN_POINT ( 'NONE',  ( 9.809058582316794173, -23.27327832286945153, 2.298404588716537411 ) ) ;
#12550 = CARTESIAN_POINT ( 'NONE',  ( -12.62500000000002132, -20.99999999999450395, 3.833333333368183382 ) ) ;
#12551 = DIRECTION ( 'NONE',  ( 1.000000000000000000, 0.000000000000000000, 0.000000000000000000 ) ) ;
#12552 = CARTESIAN_POINT ( 'NONE',  ( 6.996558582316793284, -22.05068747287764452, 1.749999999999998446 ) ) ;
#12553 = EDGE_CURVE ( 'NONE', #2453, #12804, #115, .T. ) ;
#12554 = CARTESIAN_POINT ( 'NONE',  ( 5.878441417683177406, -22.99999999999999645, 3.449312527122335048 ) ) ;
#12555 = CARTESIAN_POINT ( 'NONE',  ( -4.717959273841178636, -21.72818306014730183, 5.243595146365860771 ) ) ;
#12556 = ORIENTED_EDGE ( 'NONE', *, *, #4892, .F. ) ;
#12557 = CARTESIAN_POINT ( 'NONE',  ( 13.09560264576187905, 4.265433610975056133, 4.791666666666684726 ) ) ;
#12558 = CARTESIAN_POINT ( 'NONE',  ( -1.407845757905374695, -9.114917468222230923, 1.622643865078341463 ) ) ;
#12559 = ORIENTED_EDGE ( 'NONE', *, *, #2467, .T. ) ;
#12560 = PRODUCT_DEFINITION_CONTEXT ( 'detailed design', #12945, 'design' ) ;
#12561 =( BOUNDED_SURFACE ( )  B_SPLINE_SURFACE ( 3, 3, ( 
 ( #5511, #4150, #5613, #18387, #10217, #18588, #5409, #8651, #15231, #4050, #10433, #17008, #905, #10631, #7404, #1013, #5728, #18489, #15023, #10533, #2685, #16902, #11883, #9071, #11783, #3937, #18175, #16585, #2262, #10325, #6138, #2893, #18801, #10744, #19114, #17426, #17114, #7505, #13868, #7811, #17313, #4562, #20678, #1430, #9574, #10852, #14271, #2796, #10947, #20267, #2998, #7706, #1127, #6341, #17215, #18694, #9374, #4360, #12507, #3102, #6035, #4467, #14173, #5926, #12297, #11053, #15545, #9170, #12712, #9479, #1330, #4767, #1225, #7600, #11152, #9269, #12603, #17522, #20580, #15849, #13967, #1528, #20372, #12407, #3203, #15748 ),
 ( #15641, #14074, #20482, #18905, #6233, #19006, #4662, #7907, #16267, #8121, #375, #5177, #2046, #11247, #477, #11350, #11556, #4868, #1837, #8319, #14382, #260, #8009, #18045, #8222, #1935, #19524, #17936, #12912, #1629, #9680, #3605, #17841, #6651, #6851, #9986, #14798, #14585, #13222, #16367, #13021, #8431, #9886, #19619, #5277, #3717, #16066, #14693, #11653, #6758, #3298, #19424, #17626, #13127, #165, #15947, #65, #6451, #5081, #12815, #19214, #11457, #17741, #1739, #14488, #3405, #6548, #19315, #3506, #4971, #9787, #16173, #2239, #15206, #20036, #573, #15105, #18560, #18358, #16777, #10295, #8934, #14895, #11760, #8627, #8737 ),
 ( #5698, #7168, #16564, #2446, #782, #13531, #678, #985, #10095, #5487, #5590, #10406, #15305, #18151, #11860, #10194, #882, #2343, #2547, #19834, #14997, #20141, #16470, #19933, #8838, #7267, #7373, #11961, #2143, #13737, #13325, #5801, #7065, #3915, #13428, #13627, #6953, #16667, #12172, #10506, #3816, #4021, #18253, #8525, #19724, #5385, #12072, #18462, #4125, #16876, #1501, #6112, #15824, #4633, #20556, #4536, #2866, #5899, #13938, #17394, #18875, #9144, #14045, #6308, #15514, #16978, #1404, #20455, #3077, #9243, #6004, #1198, #13838, #7882, #6207, #20241, #10605, #2655, #10921, #12482, #7676, #9452, #17285, #12682, #20340, #14242 ),
 ( #2968, #10824, #4224, #20649, #12379, #1097, #9344, #7477, #15613, #12576, #7575, #18774, #15721, #9042, #15414, #14149, #18663, #12269, #4332, #18977, #4439, #10714, #17088, #2766, #17188, #1296, #7786, #11026, #19396, #14667, #4843, #347, #1599, #7978, #15054, #8196, #14562, #3483, #5054, #8098, #1811, #11431, #6525, #3578, #236, #16612, #737, #6624, #9858, #8683, #17816, #15922, #8293, #17911, #19500, #6424, #14461, #19292, #3380, #12994, #7120, #14352, #1712, #37, #6732, #16243, #1911, #19083, #13099, #11224, #12787, #5153, #11532, #19189, #4944, #17600, #9959, #4740, #3273, #2291, #11324, #17711, #9651, #11126, #17496, #16036 ),
 ( #3176, #141, #9550, #12888, #9761, #16146, #17038, #12327, #20093, #18723, #7529, #10561, #20295, #7431, #5952, #4392, #15569, #7219, #5857, #17142, #12227, #836, #5756, #2401, #18617, #18415, #1252, #2717, #4279, #2603, #2821, #13485, #18518, #8891, #19983, #10773, #935, #5644, #8792, #1047, #8992, #19886, #13792, #12018, #10663, #9097, #3966, #4179, #5542, #20197, #15469, #13682, #9194, #18302, #15160, #4077, #12126, #10354, #11912, #13581, #1152, #16931, #10463, #13893, #15364, #16728, #16832, #2496, #15258, #7321, #3130, #7930, #12840, #9297, #3028, #7739, #12741, #20605, #94, #17345, #14102, #17654, #7627, #6257, #20709, #19144 ),
 ( #11273, #10877, #19244, #6165, #1457, #18930, #6371, #18829, #7836, #4894, #8044, #1356, #4691, #9405, #3327, #20403, #12434, #15777, #13994, #9599, #14410, #9709, #6480, #2920, #16096, #14198, #3228, #17241, #12631, #4797, #6066, #19036, #4491, #15672, #11081, #14297, #11178, #17552, #4587, #20511, #17452, #15977, #9504, #12532, #15877, #10975, #1552, #1659, #6880, #11789, #14826, #19344, #11680, #601, #2169, #9814, #11488, #1966, #6784, #11584, #10222, #4999, #5108, #11378, #18078, #16396, #8458, #1765, #5206, #14613, #16200, #10125, #500, #17768, #8349, #3436, #14923, #8152, #291, #19647, #14724, #402, #1865, #6987, #14515, #8247 ),
 ( #18180, #3635, #13356, #8553, #3745, #2074, #13154, #6681, #17867, #19756, #13249, #13050, #17964, #3842, #19451, #192, #5306, #10017, #5416, #19551, #3537, #9913, #16294, #6575, #16497, #12940, #2267, #8656, #2579, #12105, #20069, #15448, #16908, #4366, #5620, #9077, #5516, #5734, #15028, #18494, #2476, #16590, #1132, #11994, #13460, #4156, #19864, #7296, #18593, #813, #13559, #8964, #709, #7095, #5834, #10330, #11888, #7510, #12203, #16808, #13873, #16699, #2377, #5931, #19960, #7409, #12304, #15338, #4257, #8767, #10638, #18280, #3943, #18700, #10538, #1019, #13771, #20174, #18392, #4055, #15138, #7197, #10439, #8868, #17013, #2690 ) ),
 .UNSPECIFIED., .T., .F., .F. ) 
 B_SPLINE_SURFACE_WITH_KNOTS ( ( 4, 3, 4 ),
 ( 4, 2, 2, 2, 2, 2, 2, 2, 2, 2, 2, 2, 2, 2, 2, 2, 2, 2, 2, 2, 2, 2, 2, 2, 2, 2, 2, 2, 2, 2, 2, 2, 2, 2, 2, 2, 2, 2, 2, 2, 2, 2, 4 ),
 ( 0.000000000000000000, 0.5000000000000000000, 1.000000000000000000 ),
 ( 0.000000000000000000, 0.03481082764294501225, 0.05122453910963481460, 0.05943139484297971231, 0.06353482270965216117, 0.06763825057632461002, 0.07081696859385246123, 0.07399568661138031245, 0.08035312264643601488, 0.09306799471654741973, 0.1057828667866588246, 0.1121403028217145270, 0.1153190208392423644, 0.1184977388567702156, 0.1214804596100246270, 0.1244631803632790246, 0.1304286218697878197, 0.1423595048828054099, 0.1662212709088405904, 0.2139448029609109514, 0.3093918670650516733, 0.5002859952733331728, 0.6911801234816146167, 0.7866271875857553386, 0.8343507196378256996, 0.8582124856638608801, 0.8701433686768784703, 0.8761088101833873765, 0.8790915309366418295, 0.8820742516898961716, 0.8853411830926052328, 0.8886081144953141830, 0.8951419773007323055, 0.9082097029115685505, 0.9212774285224047954, 0.9278112913278229179, 0.9310782227305318681, 0.9343451541332409294, 0.9384485819999133227, 0.9425520098665858271, 0.9507588655999306138, 0.9671725770666204092, 1.000000000000000000 ),
 .UNSPECIFIED. ) 
 GEOMETRIC_REPRESENTATION_ITEM ( )  RATIONAL_B_SPLINE_SURFACE ( (
 ( 1.000000000000000000, 1.000000000000000000, 1.000000000000000000, 1.000000000000000000, 1.000000000000000000, 1.000000000000000000, 1.000000000000000000, 1.000000000000000000, 1.000000000000000000, 1.000000000000000000, 1.000000000000000000, 1.000000000000000000, 1.000000000000000000, 1.000000000000000000, 1.000000000000000000, 1.000000000000000000, 1.000000000000000000, 1.000000000000000000, 1.000000000000000000, 1.000000000000000000, 1.000000000000000000, 1.000000000000000000, 1.000000000000000000, 1.000000000000000000, 1.000000000000000000, 1.000000000000000000, 1.000000000000000000, 1.000000000000000000, 1.000000000000000000, 1.000000000000000000, 1.000000000000000000, 1.000000000000000000, 1.000000000000000000, 1.000000000000000000, 1.000000000000000000, 1.000000000000000000, 1.000000000000000000, 1.000000000000000000, 1.000000000000000000, 1.000000000000000000, 1.000000000000000000, 1.000000000000000000, 1.000000000000000000, 1.000000000000000000, 1.000000000000000000, 1.000000000000000000, 1.000000000000000000, 1.000000000000000000, 1.000000000000000000, 1.000000000000000000, 1.000000000000000000, 1.000000000000000000, 1.000000000000000000, 1.000000000000000000, 1.000000000000000000, 1.000000000000000000, 1.000000000000000000, 1.000000000000000000, 1.000000000000000000, 1.000000000000000000, 1.000000000000000000, 1.000000000000000000, 1.000000000000000000, 1.000000000000000000, 1.000000000000000000, 1.000000000000000000, 1.000000000000000000, 1.000000000000000000, 1.000000000000000000, 1.000000000000000000, 1.000000000000000000, 1.000000000000000000, 1.000000000000000000, 1.000000000000000000, 1.000000000000000000, 1.000000000000000000, 1.000000000000000000, 1.000000000000000000, 1.000000000000000000, 1.000000000000000000, 1.000000000000000000, 1.000000000000000000, 1.000000000000000000, 1.000000000000000000, 1.000000000000000000, 1.000000000000000000),
 ( 0.3333333333333333703, 0.3333333333333333703, 0.3333333333333333703, 0.3333333333333333703, 0.3333333333333333703, 0.3333333333333333703, 0.3333333333333333703, 0.3333333333333333703, 0.3333333333333333703, 0.3333333333333333703, 0.3333333333333333703, 0.3333333333333333703, 0.3333333333333333703, 0.3333333333333333703, 0.3333333333333333703, 0.3333333333333333703, 0.3333333333333333703, 0.3333333333333333703, 0.3333333333333333703, 0.3333333333333333703, 0.3333333333333333703, 0.3333333333333333703, 0.3333333333333333703, 0.3333333333333333703, 0.3333333333333333703, 0.3333333333333333703, 0.3333333333333333703, 0.3333333333333333703, 0.3333333333333333703, 0.3333333333333333703, 0.3333333333333333703, 0.3333333333333333703, 0.3333333333333333703, 0.3333333333333333703, 0.3333333333333333703, 0.3333333333333333703, 0.3333333333333333703, 0.3333333333333333703, 0.3333333333333333703, 0.3333333333333333703, 0.3333333333333333703, 0.3333333333333333703, 0.3333333333333333703, 0.3333333333333333703, 0.3333333333333333703, 0.3333333333333333703, 0.3333333333333333703, 0.3333333333333333703, 0.3333333333333333703, 0.3333333333333333703, 0.3333333333333333703, 0.3333333333333333703, 0.3333333333333333703, 0.3333333333333333703, 0.3333333333333333703, 0.3333333333333333703, 0.3333333333333333703, 0.3333333333333333703, 0.3333333333333333703, 0.3333333333333333703, 0.3333333333333333703, 0.3333333333333333703, 0.3333333333333333703, 0.3333333333333333703, 0.3333333333333333703, 0.3333333333333333703, 0.3333333333333333703, 0.3333333333333333703, 0.3333333333333333703, 0.3333333333333333703, 0.3333333333333333703, 0.3333333333333333703, 0.3333333333333333703, 0.3333333333333333703, 0.3333333333333333703, 0.3333333333333333703, 0.3333333333333333703, 0.3333333333333333703, 0.3333333333333333703, 0.3333333333333333703, 0.3333333333333333703, 0.3333333333333333703, 0.3333333333333333703, 0.3333333333333333703, 0.3333333333333333703, 0.3333333333333333703),
 ( 0.3333333333333333703, 0.3333333333333333703, 0.3333333333333333703, 0.3333333333333333703, 0.3333333333333333703, 0.3333333333333333703, 0.3333333333333333703, 0.3333333333333333703, 0.3333333333333333703, 0.3333333333333333703, 0.3333333333333333703, 0.3333333333333333703, 0.3333333333333333703, 0.3333333333333333703, 0.3333333333333333703, 0.3333333333333333703, 0.3333333333333333703, 0.3333333333333333703, 0.3333333333333333703, 0.3333333333333333703, 0.3333333333333333703, 0.3333333333333333703, 0.3333333333333333703, 0.3333333333333333703, 0.3333333333333333703, 0.3333333333333333703, 0.3333333333333333703, 0.3333333333333333703, 0.3333333333333333703, 0.3333333333333333703, 0.3333333333333333703, 0.3333333333333333703, 0.3333333333333333703, 0.3333333333333333703, 0.3333333333333333703, 0.3333333333333333703, 0.3333333333333333703, 0.3333333333333333703, 0.3333333333333333703, 0.3333333333333333703, 0.3333333333333333703, 0.3333333333333333703, 0.3333333333333333703, 0.3333333333333333703, 0.3333333333333333703, 0.3333333333333333703, 0.3333333333333333703, 0.3333333333333333703, 0.3333333333333333703, 0.3333333333333333703, 0.3333333333333333703, 0.3333333333333333703, 0.3333333333333333703, 0.3333333333333333703, 0.3333333333333333703, 0.3333333333333333703, 0.3333333333333333703, 0.3333333333333333703, 0.3333333333333333703, 0.3333333333333333703, 0.3333333333333333703, 0.3333333333333333703, 0.3333333333333333703, 0.3333333333333333703, 0.3333333333333333703, 0.3333333333333333703, 0.3333333333333333703, 0.3333333333333333703, 0.3333333333333333703, 0.3333333333333333703, 0.3333333333333333703, 0.3333333333333333703, 0.3333333333333333703, 0.3333333333333333703, 0.3333333333333333703, 0.3333333333333333703, 0.3333333333333333703, 0.3333333333333333703, 0.3333333333333333703, 0.3333333333333333703, 0.3333333333333333703, 0.3333333333333333703, 0.3333333333333333703, 0.3333333333333333703, 0.3333333333333333703, 0.3333333333333333703),
 ( 1.000000000000000000, 1.000000000000000000, 1.000000000000000000, 1.000000000000000000, 1.000000000000000000, 1.000000000000000000, 1.000000000000000000, 1.000000000000000000, 1.000000000000000000, 1.000000000000000000, 1.000000000000000000, 1.000000000000000000, 1.000000000000000000, 1.000000000000000000, 1.000000000000000000, 1.000000000000000000, 1.000000000000000000, 1.000000000000000000, 1.000000000000000000, 1.000000000000000000, 1.000000000000000000, 1.000000000000000000, 1.000000000000000000, 1.000000000000000000, 1.000000000000000000, 1.000000000000000000, 1.000000000000000000, 1.000000000000000000, 1.000000000000000000, 1.000000000000000000, 1.000000000000000000, 1.000000000000000000, 1.000000000000000000, 1.000000000000000000, 1.000000000000000000, 1.000000000000000000, 1.000000000000000000, 1.000000000000000000, 1.000000000000000000, 1.000000000000000000, 1.000000000000000000, 1.000000000000000000, 1.000000000000000000, 1.000000000000000000, 1.000000000000000000, 1.000000000000000000, 1.000000000000000000, 1.000000000000000000, 1.000000000000000000, 1.000000000000000000, 1.000000000000000000, 1.000000000000000000, 1.000000000000000000, 1.000000000000000000, 1.000000000000000000, 1.000000000000000000, 1.000000000000000000, 1.000000000000000000, 1.000000000000000000, 1.000000000000000000, 1.000000000000000000, 1.000000000000000000, 1.000000000000000000, 1.000000000000000000, 1.000000000000000000, 1.000000000000000000, 1.000000000000000000, 1.000000000000000000, 1.000000000000000000, 1.000000000000000000, 1.000000000000000000, 1.000000000000000000, 1.000000000000000000, 1.000000000000000000, 1.000000000000000000, 1.000000000000000000, 1.000000000000000000, 1.000000000000000000, 1.000000000000000000, 1.000000000000000000, 1.000000000000000000, 1.000000000000000000, 1.000000000000000000, 1.000000000000000000, 1.000000000000000000, 1.000000000000000000),
 ( 0.3333333333333333703, 0.3333333333333333703, 0.3333333333333333703, 0.3333333333333333703, 0.3333333333333333703, 0.3333333333333333703, 0.3333333333333333703, 0.3333333333333333703, 0.3333333333333333703, 0.3333333333333333703, 0.3333333333333333703, 0.3333333333333333703, 0.3333333333333333703, 0.3333333333333333703, 0.3333333333333333703, 0.3333333333333333703, 0.3333333333333333703, 0.3333333333333333703, 0.3333333333333333703, 0.3333333333333333703, 0.3333333333333333703, 0.3333333333333333703, 0.3333333333333333703, 0.3333333333333333703, 0.3333333333333333703, 0.3333333333333333703, 0.3333333333333333703, 0.3333333333333333703, 0.3333333333333333703, 0.3333333333333333703, 0.3333333333333333703, 0.3333333333333333703, 0.3333333333333333703, 0.3333333333333333703, 0.3333333333333333703, 0.3333333333333333703, 0.3333333333333333703, 0.3333333333333333703, 0.3333333333333333703, 0.3333333333333333703, 0.3333333333333333703, 0.3333333333333333703, 0.3333333333333333703, 0.3333333333333333703, 0.3333333333333333703, 0.3333333333333333703, 0.3333333333333333703, 0.3333333333333333703, 0.3333333333333333703, 0.3333333333333333703, 0.3333333333333333703, 0.3333333333333333703, 0.3333333333333333703, 0.3333333333333333703, 0.3333333333333333703, 0.3333333333333333703, 0.3333333333333333703, 0.3333333333333333703, 0.3333333333333333703, 0.3333333333333333703, 0.3333333333333333703, 0.3333333333333333703, 0.3333333333333333703, 0.3333333333333333703, 0.3333333333333333703, 0.3333333333333333703, 0.3333333333333333703, 0.3333333333333333703, 0.3333333333333333703, 0.3333333333333333703, 0.3333333333333333703, 0.3333333333333333703, 0.3333333333333333703, 0.3333333333333333703, 0.3333333333333333703, 0.3333333333333333703, 0.3333333333333333703, 0.3333333333333333703, 0.3333333333333333703, 0.3333333333333333703, 0.3333333333333333703, 0.3333333333333333703, 0.3333333333333333703, 0.3333333333333333703, 0.3333333333333333703, 0.3333333333333333703),
 ( 0.3333333333333333703, 0.3333333333333333703, 0.3333333333333333703, 0.3333333333333333703, 0.3333333333333333703, 0.3333333333333333703, 0.3333333333333333703, 0.3333333333333333703, 0.3333333333333333703, 0.3333333333333333703, 0.3333333333333333703, 0.3333333333333333703, 0.3333333333333333703, 0.3333333333333333703, 0.3333333333333333703, 0.3333333333333333703, 0.3333333333333333703, 0.3333333333333333703, 0.3333333333333333703, 0.3333333333333333703, 0.3333333333333333703, 0.3333333333333333703, 0.3333333333333333703, 0.3333333333333333703, 0.3333333333333333703, 0.3333333333333333703, 0.3333333333333333703, 0.3333333333333333703, 0.3333333333333333703, 0.3333333333333333703, 0.3333333333333333703, 0.3333333333333333703, 0.3333333333333333703, 0.3333333333333333703, 0.3333333333333333703, 0.3333333333333333703, 0.3333333333333333703, 0.3333333333333333703, 0.3333333333333333703, 0.3333333333333333703, 0.3333333333333333703, 0.3333333333333333703, 0.3333333333333333703, 0.3333333333333333703, 0.3333333333333333703, 0.3333333333333333703, 0.3333333333333333703, 0.3333333333333333703, 0.3333333333333333703, 0.3333333333333333703, 0.3333333333333333703, 0.3333333333333333703, 0.3333333333333333703, 0.3333333333333333703, 0.3333333333333333703, 0.3333333333333333703, 0.3333333333333333703, 0.3333333333333333703, 0.3333333333333333703, 0.3333333333333333703, 0.3333333333333333703, 0.3333333333333333703, 0.3333333333333333703, 0.3333333333333333703, 0.3333333333333333703, 0.3333333333333333703, 0.3333333333333333703, 0.3333333333333333703, 0.3333333333333333703, 0.3333333333333333703, 0.3333333333333333703, 0.3333333333333333703, 0.3333333333333333703, 0.3333333333333333703, 0.3333333333333333703, 0.3333333333333333703, 0.3333333333333333703, 0.3333333333333333703, 0.3333333333333333703, 0.3333333333333333703, 0.3333333333333333703, 0.3333333333333333703, 0.3333333333333333703, 0.3333333333333333703, 0.3333333333333333703, 0.3333333333333333703),
 ( 1.000000000000000000, 1.000000000000000000, 1.000000000000000000, 1.000000000000000000, 1.000000000000000000, 1.000000000000000000, 1.000000000000000000, 1.000000000000000000, 1.000000000000000000, 1.000000000000000000, 1.000000000000000000, 1.000000000000000000, 1.000000000000000000, 1.000000000000000000, 1.000000000000000000, 1.000000000000000000, 1.000000000000000000, 1.000000000000000000, 1.000000000000000000, 1.000000000000000000, 1.000000000000000000, 1.000000000000000000, 1.000000000000000000, 1.000000000000000000, 1.000000000000000000, 1.000000000000000000, 1.000000000000000000, 1.000000000000000000, 1.000000000000000000, 1.000000000000000000, 1.000000000000000000, 1.000000000000000000, 1.000000000000000000, 1.000000000000000000, 1.000000000000000000, 1.000000000000000000, 1.000000000000000000, 1.000000000000000000, 1.000000000000000000, 1.000000000000000000, 1.000000000000000000, 1.000000000000000000, 1.000000000000000000, 1.000000000000000000, 1.000000000000000000, 1.000000000000000000, 1.000000000000000000, 1.000000000000000000, 1.000000000000000000, 1.000000000000000000, 1.000000000000000000, 1.000000000000000000, 1.000000000000000000, 1.000000000000000000, 1.000000000000000000, 1.000000000000000000, 1.000000000000000000, 1.000000000000000000, 1.000000000000000000, 1.000000000000000000, 1.000000000000000000, 1.000000000000000000, 1.000000000000000000, 1.000000000000000000, 1.000000000000000000, 1.000000000000000000, 1.000000000000000000, 1.000000000000000000, 1.000000000000000000, 1.000000000000000000, 1.000000000000000000, 1.000000000000000000, 1.000000000000000000, 1.000000000000000000, 1.000000000000000000, 1.000000000000000000, 1.000000000000000000, 1.000000000000000000, 1.000000000000000000, 1.000000000000000000, 1.000000000000000000, 1.000000000000000000, 1.000000000000000000, 1.000000000000000000, 1.000000000000000000, 1.000000000000000000) ) ) 
 REPRESENTATION_ITEM ( '' )  SURFACE ( )  );
#12562 = ORIENTED_EDGE ( 'NONE', *, *, #14847, .F. ) ;
#12563 = FACE_OUTER_BOUND ( 'NONE', #12613, .T. ) ;
#12564 = DIRECTION ( 'NONE',  ( -1.000000000000000000, 4.625929269271477434E-15, 0.000000000000000000 ) ) ;
#12565 = CARTESIAN_POINT ( 'NONE',  ( -3.257364212367626966, -9.501732542047829355, 2.664600686199549706 ) ) ;
#12566 = CARTESIAN_POINT ( 'NONE',  ( -13.83544900551672185, 3.002674778589386140, 5.971513032956590195 ) ) ;
#12567 = ADVANCED_FACE ( 'NONE', ( #3152 ), #18851, .T. ) ;
#12568 = DIRECTION ( 'NONE',  ( 0.000000000000000000, 0.000000000000000000, -1.000000000000000000 ) ) ;
#12569 = LINE ( 'NONE', #15816, #4524 ) ;
#12570 = CARTESIAN_POINT ( 'NONE',  ( 10.27780858231679417, -20.27099543870833642, 2.724438792969431589 ) ) ;
#12571 = CARTESIAN_POINT ( 'NONE',  ( -9.999999999999996447, -34.99999999999999289, 0.000000000000000000 ) ) ;
#12572 = CARTESIAN_POINT ( 'NONE',  ( 13.02352923685845631, -0.8742735386340954040, 6.652704579156702991 ) ) ;
#12573 = CARTESIAN_POINT ( 'NONE',  ( -5.965308582316795949, -19.47900456129164937, 4.484846433055089676 ) ) ;
#12574 = CARTESIAN_POINT ( 'NONE',  ( -1.824218240560544047, -9.921717538097572842, 2.387231257717697286 ) ) ;
#12575 = VERTEX_POINT ( 'NONE', #19057 ) ;
#12576 = CARTESIAN_POINT ( 'NONE',  ( -13.37499999999998224, -20.25000000000006395, 4.416666666666681174 ) ) ;
#12577 = LINE ( 'NONE', #19085, #14728 ) ;
#12578 = EDGE_CURVE ( 'NONE', #20304, #5740, #4714, .T. ) ;
#12579 = CARTESIAN_POINT ( 'NONE',  ( 6.815941417683177406, -20.26807450282663225, 5.303608408759377113 ) ) ;
#12580 = CARTESIAN_POINT ( 'NONE',  ( -11.49655858231679595, -22.05068747287764452, 2.499999999999999112 ) ) ;
#12581 = ORIENTED_EDGE ( 'NONE', *, *, #12919, .T. ) ;
#12582 = EDGE_CURVE ( 'NONE', #19275, #12628, #4815, .T. ) ;
#12583 = CARTESIAN_POINT ( 'NONE',  ( 13.37499999999998224, -20.99999999999998934, 4.291666666666699825 ) ) ;
#12584 = CARTESIAN_POINT ( 'NONE',  ( 6.183390479346035917, 4.999999999999999112, 1.000000000000000000 ) ) ;
#12585 = DIRECTION ( 'NONE',  ( 0.000000000000000000, 1.000000000000000000, 0.000000000000000000 ) ) ;
#12586 = ORIENTED_EDGE ( 'NONE', *, *, #5615, .F. ) ;
#12587 = ORIENTED_EDGE ( 'NONE', *, *, #4935, .F. ) ;
#12588 = LINE ( 'NONE', #4751, #19794 ) ;
#12589 = VECTOR ( 'NONE', #5653, 1000.000000000000000 ) ;
#12590 = CARTESIAN_POINT ( 'NONE',  ( -5.999999999999999112, -7.500000000000047073, 8.999999999999998224 ) ) ;
#12591 = ORIENTED_EDGE ( 'NONE', *, *, #3651, .F. ) ;
#12592 = CARTESIAN_POINT ( 'NONE',  ( -4.218479777801761088, -21.67082477469113755, 4.835082305552395709 ) ) ;
#12593 = ADVANCED_FACE ( 'NONE', ( #11199 ), #12861, .F. ) ;
#12594 = CARTESIAN_POINT ( 'NONE',  ( -13.12499999999999645, 5.000000000000047073, 3.999999999999996447 ) ) ;
#12595 = CARTESIAN_POINT ( 'NONE',  ( -2.693754455098655409, -10.04853567022903782, 2.237415670251142519 ) ) ;
#12596 = CARTESIAN_POINT ( 'NONE',  ( 2.195822829018478473, -9.226849102155203042, 1.651390144731336163 ) ) ;
#12597 = CARTESIAN_POINT ( 'NONE',  ( -17.94064177244175795, 10.00000000000000000, 1.000000000000000000 ) ) ;
#12598 = PLANE ( 'NONE',  #2410 ) ;
#12599 = DIRECTION ( 'NONE',  ( 0.000000000000000000, 1.000000000000000000, -0.000000000000000000 ) ) ;
#12600 = CARTESIAN_POINT ( 'NONE',  ( 26.04469207716615031, 9.000000000000001776, 1.000000000000000000 ) ) ;
#12601 = FACE_OUTER_BOUND ( 'NONE', #17605, .T. ) ;
#12602 = CARTESIAN_POINT ( 'NONE',  ( 4.472191417683178294, -22.97900456129165292, 3.035098964749240125 ) ) ;
#12603 = CARTESIAN_POINT ( 'NONE',  ( -13.12529397354238192, 5.014845663890295846, 4.916666666666650087 ) ) ;
#12604 = CARTESIAN_POINT ( 'NONE',  ( -9.340308582316795949, -22.36352608949544418, 4.520995438708343528 ) ) ;
#12605 = CARTESIAN_POINT ( 'NONE',  ( -6.253441417683175629, -21.94931252712233061, 0.9999999999999978906 ) ) ;
#12606 = ORIENTED_EDGE ( 'NONE', *, *, #17834, .T. ) ;
#12607 = EDGE_CURVE ( 'NONE', #16994, #17840, #8059, .T. ) ;
#12608 = CARTESIAN_POINT ( 'NONE',  ( 13.07121011584135672, 3.033610849983475521, 5.236678440007632496 ) ) ;
#12609 = DIRECTION ( 'NONE',  ( 1.000000000000000000, -0.000000000000000000, 0.000000000000000000 ) ) ;
#12610 = ORIENTED_EDGE ( 'NONE', *, *, #2928, .F. ) ;
#12611 = VECTOR ( 'NONE', #2085, 1000.000000000000000 ) ;
#12612 = DIRECTION ( 'NONE',  ( 0.000000000000000000, 1.000000000000000000, 0.000000000000000000 ) ) ;
#12613 = EDGE_LOOP ( 'NONE', ( #4899, #19941, #1871, #11585, #10802, #15859 ) ) ;
#12614 = CARTESIAN_POINT ( 'NONE',  ( 2.559937518207947793, -9.746075135043517079, 2.534737762559237773 ) ) ;
#12615 = VECTOR ( 'NONE', #19367, 1000.000000000000000 ) ;
#12616 = ORIENTED_EDGE ( 'NONE', *, *, #3188, .T. ) ;
#12617 = CARTESIAN_POINT ( 'NONE',  ( 11.78469141768317563, -23.77099543870834353, 4.174186261275251830 ) ) ;
#12618 = EDGE_CURVE ( 'NONE', #9549, #15974, #17367, .T. ) ;
#12619 = CARTESIAN_POINT ( 'NONE',  ( -4.000000000000000000, -8.500000000000000000, 1.000000000000000000 ) ) ;
#12620 = CARTESIAN_POINT ( 'NONE',  ( -1.903957340438703572, -10.27085516675799148, 2.476896775482616331 ) ) ;
#12621 = CARTESIAN_POINT ( 'NONE',  ( 2.311130159782011972, 9.000000000000001776, 0.000000000000000000 ) ) ;
#12622 = CARTESIAN_POINT ( 'NONE',  ( -12.52780858231679595, -23.72900456129165292, 4.275561207030568411 ) ) ;
#12623 = VECTOR ( 'NONE', #13348, 1000.000000000000000 ) ;
#12624 = CARTESIAN_POINT ( 'NONE',  ( 7.619520639128047002, 0.000000000000000000, 0.000000000000000000 ) ) ;
#12625 = CARTESIAN_POINT ( 'NONE',  ( 4.940941417683177406, -20.19639159124061933, 1.768074502826635586 ) ) ;
#12626 = DIRECTION ( 'NONE',  ( -1.000000000000000000, 0.000000000000000000, 0.000000000000000000 ) ) ;
#12627 = CARTESIAN_POINT ( 'NONE',  ( -9.628441417683177406, -20.24999999999999289, 3.550687472877664952 ) ) ;
#12628 = VERTEX_POINT ( 'NONE', #14219 ) ;
#12629 = CARTESIAN_POINT ( 'NONE',  ( 9.152808582316794173, -21.22443879296942626, 5.229004561291659137 ) ) ;
#12630 = CARTESIAN_POINT ( 'NONE',  ( -5.381197846483055436, -14.00000000000000000, 2.000000000000000000 ) ) ;
#12631 = CARTESIAN_POINT ( 'NONE',  ( -12.66024186180961308, -19.22028597861421417, 6.258173329156003106 ) ) ;
#12632 = ORIENTED_EDGE ( 'NONE', *, *, #13629, .T. ) ;
#12633 = CARTESIAN_POINT ( 'NONE',  ( 9.152808582316794173, -21.22443879296942626, 5.229004561291659137 ) ) ;
#12634 = LINE ( 'NONE', #17147, #12653 ) ;
#12635 = ORIENTED_EDGE ( 'NONE', *, *, #15979, .F. ) ;
#12636 = DIRECTION ( 'NONE',  ( 1.000000000000000000, 0.000000000000000000, 0.000000000000000000 ) ) ;
#12637 = ORIENTED_EDGE ( 'NONE', *, *, #19226, .F. ) ;
#12638 = VECTOR ( 'NONE', #13832, 1000.000000000000227 ) ;
#12639 = DIRECTION ( 'NONE',  ( 0.1736481776669295263, -0.9848077530122082424, 0.000000000000000000 ) ) ;
#12640 = VECTOR ( 'NONE', #11693, 1000.000000000000000 ) ;
#12641 = ORIENTED_EDGE ( 'NONE', *, *, #1059, .T. ) ;
#12642 = CARTESIAN_POINT ( 'NONE',  ( -7.840308582316794173, -22.67418626127525982, 5.270995438708342640 ) ) ;
#12643 = LINE ( 'NONE', #14116, #17632 ) ;
#12644 = CYLINDRICAL_SURFACE ( 'NONE', #10822, 0.2500000000000002220 ) ;
#12645 = CARTESIAN_POINT ( 'NONE',  ( 2.282685604506861754, -11.80366834561962364, 2.120553820834011116 ) ) ;
#12646 = EDGE_CURVE ( 'NONE', #4544, #12022, #6280, .T. ) ;
#12647 = CARTESIAN_POINT ( 'NONE',  ( -9.689245429134309973, 0.000000000000000000, 1.000000000000000000 ) ) ;
#12648 = CARTESIAN_POINT ( 'NONE',  ( -13.47561960997282071, -14.41870969638424071, 4.846833296715798767 ) ) ;
#12649 = AXIS2_PLACEMENT_3D ( 'NONE', #3286, #15936, #1616 ) ;
#12650 = VECTOR ( 'NONE', #17440, 1000.000000000000227 ) ;
#12651 = CARTESIAN_POINT ( 'NONE',  ( 9.246558582316794173, -21.94931252712234482, 5.250000000000000888 ) ) ;
#12652 = CARTESIAN_POINT ( 'NONE',  ( -12.65986935584910000, -19.23909752961862907, 6.257782094979345899 ) ) ;
#12653 = VECTOR ( 'NONE', #17243, 1000.000000000000000 ) ;
#12654 = DIRECTION ( 'NONE',  ( -0.000000000000000000, -0.000000000000000000, -1.000000000000000000 ) ) ;
#12655 = CARTESIAN_POINT ( 'NONE',  ( 5.309058582316794173, -23.27327832286945153, 2.298404588716537411 ) ) ;
#12656 = CARTESIAN_POINT ( 'NONE',  ( 6.253441417683175629, -21.94931252712233061, 2.499999999999999112 ) ) ;
#12657 = CARTESIAN_POINT ( 'NONE',  ( -10.94094141768317741, -20.72672167713052715, 2.298404588716546293 ) ) ;
#12658 = ORIENTED_EDGE ( 'NONE', *, *, #7111, .T. ) ;
#12659 = CARTESIAN_POINT ( 'NONE',  ( 13.37732542738919328, -19.38256591684242025, 4.710253041318374301 ) ) ;
#12660 = PLANE ( 'NONE',  #656 ) ;
#12661 = ORIENTED_EDGE ( 'NONE', *, *, #14786, .T. ) ;
#12662 = VERTEX_POINT ( 'NONE', #19166 ) ;
#12663 = CARTESIAN_POINT ( 'NONE',  ( -13.49999999999998401, -19.49999999999999645, 1.000000000000000000 ) ) ;
#12664 = VECTOR ( 'NONE', #5097, 1000.000000000000000 ) ;
#12665 = AXIS2_PLACEMENT_3D ( 'NONE', #15740, #12089, #18481 ) ;
#12666 = CARTESIAN_POINT ( 'NONE',  ( -13.12529418130016445, 5.014856155665242454, 4.958178834604180629 ) ) ;
#12667 = AXIS2_PLACEMENT_3D ( 'NONE', #556, #16547, #8608 ) ;
#12668 = PRODUCT_DEFINITION_SHAPE ( 'NONE', 'NONE',  #20720 ) ;
#12669 = CARTESIAN_POINT ( 'NONE',  ( -3.779650890485476200, -11.92851441922421607, 2.537846752097290715 ) ) ;
#12670 = DIRECTION ( 'NONE',  ( -0.000000000000000000, -0.000000000000000000, -1.000000000000000000 ) ) ;
#12671 = ADVANCED_FACE ( 'NONE', ( #9620 ), #6704, .F. ) ;
#12672 = CARTESIAN_POINT ( 'NONE',  ( 2.768424032093183662, -10.00067216410020166, 1.850123365707658785 ) ) ;
#12673 = CARTESIAN_POINT ( 'NONE',  ( -12.62499999999998224, -20.24999999999991829, 4.333333333333343695 ) ) ;
#12674 = DIRECTION ( 'NONE',  ( -0.000000000000000000, -0.000000000000000000, -1.000000000000000000 ) ) ;
#12675 = DIRECTION ( 'NONE',  ( 0.1736481776669309696, 0.9848077530122080203, 0.000000000000000000 ) ) ;
#12676 = CARTESIAN_POINT ( 'NONE',  ( 13.15492785973632017, 5.761356916681801721, 5.116543252045025802 ) ) ;
#12677 = CARTESIAN_POINT ( 'NONE',  ( -11.50344141768317741, -22.05068747287766229, 6.000000000000001776 ) ) ;
#12678 = CARTESIAN_POINT ( 'NONE',  ( -2.044552395631970665, -10.13052631352519306, 1.690857522621936226 ) ) ;
#12679 = EDGE_CURVE ( 'NONE', #9180, #6959, #8376, .T. ) ;
#12680 = ORIENTED_EDGE ( 'NONE', *, *, #15015, .F. ) ;
#12681 = EDGE_CURVE ( 'NONE', #8195, #10885, #7389, .T. ) ;
#12682 = CARTESIAN_POINT ( 'NONE',  ( -13.84501469867711698, 4.235742283194553259, 3.666666666666500873 ) ) ;
#12683 = LINE ( 'NONE', #6526, #3047 ) ;
#12684 = CARTESIAN_POINT ( 'NONE',  ( 8.409691417683177406, -21.01515356694492098, 6.020995438708349745 ) ) ;
#12685 =( BOUNDED_CURVE ( )  B_SPLINE_CURVE ( 3, ( #8642, #10006, #11573, #15016 ),
 .UNSPECIFIED., .F., .F. ) 
 B_SPLINE_CURVE_WITH_KNOTS ( ( 4, 4 ),
 ( 0.001172421487176120289, 0.001187255941418635012 ),
 .UNSPECIFIED. ) 
 CURVE ( )  GEOMETRIC_REPRESENTATION_ITEM ( )  RATIONAL_B_SPLINE_CURVE ( ( 0.9999999999999996669, 0.9870550161812248202, 0.9743613912715525238, 0.9619191252709827777 ) ) 
 REPRESENTATION_ITEM ( '' )  );
#12686 = CARTESIAN_POINT ( 'NONE',  ( -5.878441417683177406, -22.99999999999999645, 3.449312527122335048 ) ) ;
#12687 = PRESENTATION_LAYER_ASSIGNMENT (  '', '', ( #10367 ) ) ;
#12688 = ORIENTED_EDGE ( 'NONE', *, *, #1611, .T. ) ;
#12689 = CARTESIAN_POINT ( 'NONE',  ( 13.37499999999998224, -20.99999999999991829, 4.333333333333343695 ) ) ;
#12690 = DIRECTION ( 'NONE',  ( -0.000000000000000000, -0.000000000000000000, -1.000000000000000000 ) ) ;
#12691 = CARTESIAN_POINT ( 'NONE',  ( -22.85856191738413656, 9.000000000000001776, 0.000000000000000000 ) ) ;
#12692 = ORIENTED_EDGE ( 'NONE', *, *, #11662, .F. ) ;
#12693 = AXIS2_PLACEMENT_3D ( 'NONE', #2186, #5123, #11503 ) ;
#12694 = ORIENTED_EDGE ( 'NONE', *, *, #8750, .T. ) ;
#12695 = CARTESIAN_POINT ( 'NONE',  ( 11.00000000000000000, -19.49999999999999645, 5.000000000000000000 ) ) ;
#12696 = DIRECTION ( 'NONE',  ( -0.000000000000000000, 0.000000000000000000, -1.000000000000000000 ) ) ;
#12697 = VECTOR ( 'NONE', #19542, 1000.000000000000000 ) ;
#12698 = CARTESIAN_POINT ( 'NONE',  ( -4.250698171653726654, 10.00000000000000000, 1.000000000000000000 ) ) ;
#12699 = CARTESIAN_POINT ( 'NONE',  ( 2.203959450683124377, -9.262433282444222371, 2.410528873095051594 ) ) ;
#12700 = EDGE_CURVE ( 'NONE', #3061, #14333, #3456, .T. ) ;
#12701 = DIRECTION ( 'NONE',  ( 0.000000000000000000, 1.000000000000000000, 0.000000000000000000 ) ) ;
#12702 = CARTESIAN_POINT ( 'NONE',  ( 1.639793706121975614, -8.364901960018411131, 1.622639882261793343 ) ) ;
#12703 = DIRECTION ( 'NONE',  ( 3.469446951953611033E-15, -1.000000000000000000, 0.000000000000000000 ) ) ;
#12704 = CYLINDRICAL_SURFACE ( 'NONE', #12425, 2.999999999999999112 ) ;
#12705 = VECTOR ( 'NONE', #2794, 1000.000000000000000 ) ;
#12706 = AXIS2_PLACEMENT_3D ( 'NONE', #14071, #4248, #20479 ) ;
#12707 = CARTESIAN_POINT ( 'NONE',  ( 0.3749999999999968914, 0.000000000000000000, 1.000000000000000000 ) ) ;
#12708 = CARTESIAN_POINT ( 'NONE',  ( 2.311130159782011972, 4.999999999999999112, 1.000000000000000000 ) ) ;
#12709 = LINE ( 'NONE', #13018, #6389 ) ;
#12710 = CARTESIAN_POINT ( 'NONE',  ( -2.602174906157317835, -9.976397331638239052, 2.593889103792902606 ) ) ;
#12711 = CARTESIAN_POINT ( 'NONE',  ( 5.222191417683177406, -21.02099543870834353, 3.964901035250761208 ) ) ;
#12712 = CARTESIAN_POINT ( 'NONE',  ( -13.12270769621861355, 4.884238659038159902, 5.513847264053151065 ) ) ;
#12713 = CARTESIAN_POINT ( 'NONE',  ( -6.809058582316796837, -22.74294823697954016, 2.828734674606448785 ) ) ;
#12714 = CARTESIAN_POINT ( 'NONE',  ( -11.97219141768317563, -23.72900456129165292, 2.724438792969417822 ) ) ;
#12715 = ORIENTED_EDGE ( 'NONE', *, *, #17145, .T. ) ;
#12716 = CARTESIAN_POINT ( 'NONE',  ( 13.09123688038123490, 4.044962459253448550, 5.255034774807352704 ) ) ;
#12717 = CARTESIAN_POINT ( 'NONE',  ( 0.000000000000000000, 11.64110105645932691, 10.00000000000000000 ) ) ;
#12718 = EDGE_LOOP ( 'NONE', ( #8258, #10273, #406, #19290, #7983, #1909, #16522, #6910, #13464, #12106 ) ) ;
#12719 = ADVANCED_FACE ( 'NONE', ( #7010 ), #18203, .F. ) ;
#12720 = LINE ( 'NONE', #11565, #19695 ) ;
#12721 = ORIENTED_EDGE ( 'NONE', *, *, #17948, .F. ) ;
#12722 = LINE ( 'NONE', #19125, #20131 ) ;
#12723 = AXIS2_PLACEMENT_3D ( 'NONE', #6804, #11508, #13380 ) ;
#12724 = VECTOR ( 'NONE', #62, 1000.000000000000000 ) ;
#12725 = AXIS2_PLACEMENT_3D ( 'NONE', #11098, #19160, #17676 ) ;
#12726 = VERTEX_POINT ( 'NONE', #11603 ) ;
#12727 = CARTESIAN_POINT ( 'NONE',  ( 11.97219141768317563, -23.72900456129164937, 2.724438792969417378 ) ) ;
#12728 = CARTESIAN_POINT ( 'NONE',  ( -20.49999999999998224, -21.99999999999999645, 11.00000000000000178 ) ) ;
#12729 = ADVANCED_FACE ( 'NONE', ( #622 ), #16219, .T. ) ;
#12730 = ADVANCED_FACE ( 'NONE', ( #16518 ), #5024, .T. ) ;
#12731 = CARTESIAN_POINT ( 'NONE',  ( -1.904508877737772998, -9.138371295333994837, 2.378667276417936627 ) ) ;
#12732 = CARTESIAN_POINT ( 'NONE',  ( 0.000000000000000000, 9.000000000000001776, 0.000000000000000000 ) ) ;
#12733 = DIRECTION ( 'NONE',  ( 1.000000000000000000, -0.000000000000000000, -0.000000000000000000 ) ) ;
#12734 = CARTESIAN_POINT ( 'NONE',  ( 6.722191417683176518, -19.52099543870834353, 4.586221378810406257 ) ) ;
#12735 = CARTESIAN_POINT ( 'NONE',  ( 0.000000000000000000, 10.00000000000000000, 1.000000000000000000 ) ) ;
#12736 = CARTESIAN_POINT ( 'NONE',  ( -5.878441417683177406, -23.74999999999999645, 3.449312527122335492 ) ) ;
#12737 = VECTOR ( 'NONE', #20644, 1000.000000000000000 ) ;
#12738 = ORIENTED_EDGE ( 'NONE', *, *, #15346, .T. ) ;
#12739 = CARTESIAN_POINT ( 'NONE',  ( 7.090308582316794173, -21.32581373872472597, 1.729004561291657582 ) ) ;
#12740 = CARTESIAN_POINT ( 'NONE',  ( 25.04469207716615031, 0.000000000000000000, 1.000000000000000000 ) ) ;
#12741 = CARTESIAN_POINT ( 'NONE',  ( -13.90439735423812273, 5.734566389025032684, 4.916666666666649199 ) ) ;
#12742 = ADVANCED_FACE ( 'NONE', ( #3555 ), #11403, .T. ) ;
#12743 = LINE ( 'NONE', #12436, #15288 ) ;
#12744 = CARTESIAN_POINT ( 'NONE',  ( 21.17243175760212637, 4.999999999999999112, 1.000000000000000000 ) ) ;
#12745 = ORIENTED_EDGE ( 'NONE', *, *, #19968, .F. ) ;
#12746 = CARTESIAN_POINT ( 'NONE',  ( -3.499999999999998668, -19.50000000000000000, 1.000000000000000000 ) ) ;
#12747 =( NAMED_UNIT ( * ) SI_UNIT ( $, .STERADIAN. ) SOLID_ANGLE_UNIT ( ) );
#12748 = ORIENTED_EDGE ( 'NONE', *, *, #8976, .F. ) ;
#12749 = CARTESIAN_POINT ( 'NONE',  ( -16.62779268661489951, 10.00000000000000000, 1.000000000000000000 ) ) ;
#12750 = EDGE_LOOP ( 'NONE', ( #1963, #994, #12745, #5393 ) ) ;
#12751 = CARTESIAN_POINT ( 'NONE',  ( -6.715308582316794173, -23.77099543870833998, 2.825813738724734847 ) ) ;
#12752 = VECTOR ( 'NONE', #5130, 1000.000000000000000 ) ;
#12753 = CARTESIAN_POINT ( 'NONE',  ( 12.62499999999998224, -20.24999999999998934, 4.166666666666636765 ) ) ;
#12754 = LINE ( 'NONE', #11395, #467 ) ;
#12755 = CARTESIAN_POINT ( 'NONE',  ( 2.057814715640970515, -10.20705538578787852, 1.710511717200805304 ) ) ;
#12756 = STYLED_ITEM ( 'NONE', ( #754 ), #17773 ) ;
#12757 = CARTESIAN_POINT ( 'NONE',  ( -20.00349085826861995, 0.000000000000000000, 1.000000000000000000 ) ) ;
#12758 = CARTESIAN_POINT ( 'NONE',  ( -13.83051420738022763, 3.503467472703414742, 5.232249963382380464 ) ) ;
#12759 = CARTESIAN_POINT ( 'NONE',  ( 7.465308582316795061, -20.22900456129164937, 4.174186261275266929 ) ) ;
#12760 = CARTESIAN_POINT ( 'NONE',  ( -12.67822638532683577, -18.31206754099172684, 6.277704579156187847 ) ) ;
#12761 = CARTESIAN_POINT ( 'NONE',  ( -11.99999999999999467, -17.50000000000000000, 4.000000000000000000 ) ) ;
#12762 = CARTESIAN_POINT ( 'NONE',  ( -6.527808582316795949, -24.47900456129166358, 4.586221378810390270 ) ) ;
#12763 = CARTESIAN_POINT ( 'NONE',  ( 7.465308582316795061, -20.22900456129164937, 4.174186261275266929 ) ) ;
#12764 = VECTOR ( 'NONE', #4655, 1000.000000000000000 ) ;
#12765 = ADVANCED_FACE ( 'NONE', ( #14845 ), #1888, .T. ) ;
#12766 = CARTESIAN_POINT ( 'NONE',  ( 4.190941417683176518, -22.74294823697955081, 4.171265325393542334 ) ) ;
#12767 = CARTESIAN_POINT ( 'NONE',  ( -5.222191417683177406, -20.27099543870833998, 4.275561207030583510 ) ) ;
#12768 = ORIENTED_EDGE ( 'NONE', *, *, #15152, .F. ) ;
#12769 = CARTESIAN_POINT ( 'NONE',  ( 13.84167967300649238, 4.067323486828401613, 5.231641758301140754 ) ) ;
#12770 = DIRECTION ( 'NONE',  ( 0.1351665943404306014, 0.9596796555888912339, -0.2464649070825229438 ) ) ;
#12771 = VERTEX_POINT ( 'NONE', #3767 ) ;
#12772 = VERTEX_POINT ( 'NONE', #9936 ) ;
#12773 = CARTESIAN_POINT ( 'NONE',  ( 28.94203811574921659, 16.00000000000000000, 1.000000000000000000 ) ) ;
#12774 = CARTESIAN_POINT ( 'NONE',  ( -20.92243175760212637, 0.000000000000000000, 1.000000000000000000 ) ) ;
#12775 = CARTESIAN_POINT ( 'NONE',  ( -7.500000000000000000, -20.16506350946107418, 5.000000000000000000 ) ) ;
#12776 = EDGE_CURVE ( 'NONE', #8019, #15255, #16315, .T. ) ;
#12777 = CARTESIAN_POINT ( 'NONE',  ( -3.336296098497695262, -9.936854405034125648, 2.776348673047012383 ) ) ;
#12778 = CARTESIAN_POINT ( 'NONE',  ( -0.000000000000000000, 11.64110105645932691, 0.000000000000000000 ) ) ;
#12779 = VECTOR ( 'NONE', #15501, 1000.000000000000000 ) ;
#12780 = CARTESIAN_POINT ( 'NONE',  ( 2.195822829018478473, -9.226849102155203042, 1.651390144731336163 ) ) ;
#12781 = CARTESIAN_POINT ( 'NONE',  ( -13.10557919622060652, 4.019249409169220577, 6.007898877577752650 ) ) ;
#12782 = CARTESIAN_POINT ( 'NONE',  ( 4.247260319564023945, 9.000000000000001776, 1.000000000000000000 ) ) ;
#12783 = FACE_OUTER_BOUND ( 'NONE', #18024, .T. ) ;
#12784 = CARTESIAN_POINT ( 'NONE',  ( 12.81251082758882376, -11.53070320674076576, 6.423537912489145185 ) ) ;
#12785 = CARTESIAN_POINT ( 'NONE',  ( -1.897597015127918230, -9.924601616748528699, 1.637971946730535588 ) ) ;
#12786 = ORIENTED_EDGE ( 'NONE', *, *, #6571, .F. ) ;
#12787 = CARTESIAN_POINT ( 'NONE',  ( -13.87406079471522347, 4.952570133121557028, 5.260711232101737522 ) ) ;
#12788 = DIRECTION ( 'NONE',  ( 0.000000000000000000, 0.000000000000000000, -1.000000000000000000 ) ) ;
#12789 = CARTESIAN_POINT ( 'NONE',  ( 8.784691417683177406, -24.52099543870834708, 4.484846433055073689 ) ) ;
#12790 = AXIS2_PLACEMENT_3D ( 'NONE', #9612, #15995, #16108 ) ;
#12791 = CARTESIAN_POINT ( 'NONE',  ( -11.21530858231679595, -23.02099543870833998, 3.136473910504556262 ) ) ;
#12792 = ORIENTED_EDGE ( 'NONE', *, *, #9517, .F. ) ;
#12793 = CARTESIAN_POINT ( 'NONE',  ( 12.62499999999998224, -21.00000000000006395, 4.416666666666682062 ) ) ;
#12794 = CARTESIAN_POINT ( 'NONE',  ( 13.12529418130016445, 5.014856155665242454, 4.958178834604180629 ) ) ;
#12795 = LINE ( 'NONE', #9557, #6008 ) ;
#12796 = ORIENTED_EDGE ( 'NONE', *, *, #20280, .F. ) ;
#12797 = VECTOR ( 'NONE', #15735, 1000.000000000000000 ) ;
#12798 = EDGE_CURVE ( 'NONE', #19218, #16697, #2190, .T. ) ;
#12799 = ORIENTED_EDGE ( 'NONE', *, *, #3105, .T. ) ;
#12800 = DIRECTION ( 'NONE',  ( -1.734723475976787570E-15, 1.000000000000000000, 0.000000000000000000 ) ) ;
#12801 = DIRECTION ( 'NONE',  ( 1.000000000000000000, 0.000000000000000000, -0.000000000000000000 ) ) ;
#12802 = EDGE_CURVE ( 'NONE', #4223, #13134, #11812, .T. ) ;
#12803 = ADVANCED_FACE ( 'NONE', ( #425 ), #8171, .T. ) ;
#12804 = VERTEX_POINT ( 'NONE', #5333 ) ;
#12805 = DIRECTION ( 'NONE',  ( 0.000000000000000000, 0.000000000000000000, 1.000000000000000000 ) ) ;
#12806 = DIRECTION ( 'NONE',  ( 1.000000000000000000, -0.000000000000000000, 0.000000000000000000 ) ) ;
#12807 = CARTESIAN_POINT ( 'NONE',  ( 2.512468814886674284, -13.43512376012158782, 2.539544162874482591 ) ) ;
#12808 = FACE_OUTER_BOUND ( 'NONE', #11795, .T. ) ;
#12809 = CARTESIAN_POINT ( 'NONE',  ( -15.00000000000000000, 0.000000000000000000, 1.000000000000000000 ) ) ;
#12810 = LINE ( 'NONE', #3401, #19406 ) ;
#12811 = DIRECTION ( 'NONE',  ( 0.000000000000000000, -1.000000000000000000, 0.000000000000000000 ) ) ;
#12812 = LINE ( 'NONE', #17837, #5368 ) ;
#12813 = CARTESIAN_POINT ( 'NONE',  ( -2.594671182134835163, -9.923034775318452461, 2.580184533305832861 ) ) ;
#12814 = CARTESIAN_POINT ( 'NONE',  ( 11.12155858231679595, -22.99999999999999645, 3.550687472877652073 ) ) ;
#12815 = CARTESIAN_POINT ( 'NONE',  ( -13.09080647246885576, 4.023226859705822278, 5.257958009367514229 ) ) ;
#12816 = CARTESIAN_POINT ( 'NONE',  ( -4.717959273841179524, -21.82295283170803302, 4.493595146365858994 ) ) ;
#12817 = CARTESIAN_POINT ( 'NONE',  ( -5.597191417683177406, -23.08622137881040359, 5.979004561291654696 ) ) ;
#12818 = EDGE_LOOP ( 'NONE', ( #16706, #6576, #19555, #6531 ) ) ;
#12819 = CARTESIAN_POINT ( 'NONE',  ( 13.37499994994395891, -19.50000252782794519, 4.474109982178703149 ) ) ;
#12820 = CARTESIAN_POINT ( 'NONE',  ( -26.79469207716615387, 9.000000000000001776, 1.000000000000000000 ) ) ;
#12821 = EDGE_LOOP ( 'NONE', ( #17529, #35, #4309, #99 ) ) ;
#12822 = VERTEX_POINT ( 'NONE', #8575 ) ;
#12823 = DIRECTION ( 'NONE',  ( 1.000000000000000000, 0.000000000000000000, 0.000000000000000000 ) ) ;
#12824 = EDGE_CURVE ( 'NONE', #20175, #483, #6403, .T. ) ;
#12825 = ORIENTED_EDGE ( 'NONE', *, *, #1732, .T. ) ;
#12826 = FACE_OUTER_BOUND ( 'NONE', #17505, .T. ) ;
#12827 = ORIENTED_EDGE ( 'NONE', *, *, #2628, .T. ) ;
#12828 = CARTESIAN_POINT ( 'NONE',  ( 9.440941417683177406, -20.72672167713052715, 2.298404588716546293 ) ) ;
#12829 = CARTESIAN_POINT ( 'NONE',  ( -4.315753587183824180, -21.56469153729574018, 5.194994555241421175 ) ) ;
#12830 = CARTESIAN_POINT ( 'NONE',  ( -2.579281110863027582, -9.822567596814183233, 2.554382554832406615 ) ) ;
#12831 = CARTESIAN_POINT ( 'NONE',  ( -0.000000000000000000, 10.00000000000000000, 0.000000000000000000 ) ) ;
#12832 = CARTESIAN_POINT ( 'NONE',  ( 15.50000000000002132, -26.49999999999999645, 4.000000000000000000 ) ) ;
#12833 = CARTESIAN_POINT ( 'NONE',  ( 0.000000000000000000, 4.999999999999999112, 1.000000000000000000 ) ) ;
#12834 = CARTESIAN_POINT ( 'NONE',  ( 8.128441417683175629, -20.24999999999999289, 3.550687472877664952 ) ) ;
#12835 = CARTESIAN_POINT ( 'NONE',  ( 0.000000000000000000, 16.00000000000000000, 1.000000000000000000 ) ) ;
#12836 = CARTESIAN_POINT ( 'NONE',  ( -12.53469141768317741, -20.97900456129164581, 3.136473910504570917 ) ) ;
#12837 = VERTEX_POINT ( 'NONE', #12964 ) ;
#12838 = CARTESIAN_POINT ( 'NONE',  ( 7.371558582316795949, -19.49999999999998934, 3.449312527122348371 ) ) ;
#12839 = DIRECTION ( 'NONE',  ( 3.469446951953619119E-16, -1.000000000000000000, 0.000000000000000000 ) ) ;
#12840 = CARTESIAN_POINT ( 'NONE',  ( -13.90411326029870409, 5.720219645086723759, 5.230514352905474063 ) ) ;
#12841 = ORIENTED_EDGE ( 'NONE', *, *, #959, .F. ) ;
#12842 = CARTESIAN_POINT ( 'NONE',  ( 4.687312169500632564, -21.51559725698341197, 5.182386163300427562 ) ) ;
#12843 = EDGE_CURVE ( 'NONE', #8244, #42, #11707, .T. ) ;
#12844 = DIRECTION ( 'NONE',  ( -0.000000000000000000, -0.000000000000000000, -1.000000000000000000 ) ) ;
#12845 = ADVANCED_FACE ( 'NONE', ( #8681 ), #17036, .T. ) ;
#12846 = ORIENTED_EDGE ( 'NONE', *, *, #15141, .T. ) ;
#12847 = DIRECTION ( 'NONE',  ( 0.000000000000000000, 0.000000000000000000, 1.000000000000000000 ) ) ;
#12848 =( LENGTH_UNIT ( ) NAMED_UNIT ( * ) SI_UNIT ( .MILLI., .METRE. ) );
#12849 = ORIENTED_EDGE ( 'NONE', *, *, #8607, .F. ) ;
#12850 = PLANE ( 'NONE',  #3118 ) ;
#12851 = VERTEX_POINT ( 'NONE', #15467 ) ;
#12852 = CARTESIAN_POINT ( 'NONE',  ( -5.684058582316794173, -20.79840458871652942, 2.226721677130544030 ) ) ;
#12853 = PLANE ( 'NONE',  #4925 ) ;
#12854 = DIRECTION ( 'NONE',  ( 0.000000000000000000, 1.000000000000000000, -0.000000000000000000 ) ) ;
#12855 = CARTESIAN_POINT ( 'NONE',  ( 2.050137595624097031, -10.15260257655714504, 1.696527147986202522 ) ) ;
#12856 = CARTESIAN_POINT ( 'NONE',  ( 12.64195242771744709, -19.39390240027112000, 5.496549442168085164 ) ) ;
#12857 = DIRECTION ( 'NONE',  ( -0.000000000000000000, -0.000000000000000000, -1.000000000000000000 ) ) ;
#12858 = CARTESIAN_POINT ( 'NONE',  ( -13.38269957179998038, -19.11117162410040038, 4.745921838382382241 ) ) ;
#12859 = CARTESIAN_POINT ( 'NONE',  ( 8.965308582316794173, -20.22900456129164937, 4.174186261275266929 ) ) ;
#12860 = CARTESIAN_POINT ( 'NONE',  ( -13.90439735423812273, 5.734566389025032684, 4.916666666666649199 ) ) ;
#12861 = PLANE ( 'NONE',  #10730 ) ;
#12862 = CARTESIAN_POINT ( 'NONE',  ( -10.27780858231679595, -19.52099543870833642, 2.413778621189609286 ) ) ;
#12863 = CARTESIAN_POINT ( 'NONE',  ( 4.687312169500632564, -21.51559725698341197, 5.182386163300427562 ) ) ;
#12864 = AXIS2_PLACEMENT_3D ( 'NONE', #16235, #1901, #11520 ) ;
#12865 = AXIS2_PLACEMENT_3D ( 'NONE', #14142, #20549, #20332 ) ;
#12866 = CARTESIAN_POINT ( 'NONE',  ( 7.659691417683177406, -22.36352608949543352, 2.479004561291652031 ) ) ;
#12867 = CARTESIAN_POINT ( 'NONE',  ( -6.909691417683177406, -21.32581373872474373, 5.270995438708348857 ) ) ;
#12868 = ORIENTED_EDGE ( 'NONE', *, *, #9328, .T. ) ;
#12869 = ORIENTED_EDGE ( 'NONE', *, *, #16436, .F. ) ;
#12870 = CARTESIAN_POINT ( 'NONE',  ( 13.37499999999998224, -20.25000000000006395, 4.416666666666681174 ) ) ;
#12871 = CARTESIAN_POINT ( 'NONE',  ( 0.000000000000000000, 11.64110105645932691, 10.00000000000000000 ) ) ;
#12872 = CARTESIAN_POINT ( 'NONE',  ( -10.43924542913431175, 10.00000000000000000, 1.000000000000000000 ) ) ;
#12873 = VERTEX_POINT ( 'NONE', #7118 ) ;
#12874 = VERTEX_POINT ( 'NONE', #20195 ) ;
#12875 = LINE ( 'NONE', #17380, #15455 ) ;
#12876 = CARTESIAN_POINT ( 'NONE',  ( -5.563547257480587760, 11.64110105645932691, 10.00000000000000000 ) ) ;
#12877 = DIRECTION ( 'NONE',  ( 0.000000000000000000, 1.000000000000000000, 0.000000000000000000 ) ) ;
#12878 = CARTESIAN_POINT ( 'NONE',  ( 0.000000000000000000, -9.114917468222230923, 2.372643865078340575 ) ) ;
#12879 = DIRECTION ( 'NONE',  ( -1.000000000000000000, 0.000000000000000000, 0.000000000000000000 ) ) ;
#12880 = ADVANCED_FACE ( 'NONE', ( #13891 ), #10243, .F. ) ;
#12881 = FACE_OUTER_BOUND ( 'NONE', #18476, .T. ) ;
#12882 = CARTESIAN_POINT ( 'NONE',  ( -13.10192273101908000, 3.834597916462216816, 6.003936301248457674 ) ) ;
#12883 = CARTESIAN_POINT ( 'NONE',  ( 12.52780858231679595, -23.72900456129165292, 4.275561207030568411 ) ) ;
#12884 = DIRECTION ( 'NONE',  ( 0.000000000000000000, 1.000000000000000000, 0.000000000000000000 ) ) ;
#12885 = CARTESIAN_POINT ( 'NONE',  ( 13.15498530132288479, 5.764257716805535559, 4.333333333333380999 ) ) ;
#12886 = CARTESIAN_POINT ( 'NONE',  ( -1.991511895312070957, -10.01421418592441448, 1.660986244685804136 ) ) ;
#12887 = EDGE_LOOP ( 'NONE', ( #6292, #845, #8524, #18287, #12796, #20348, #7539, #5759, #3664, #14153 ) ) ;
#12888 = CARTESIAN_POINT ( 'NONE',  ( -13.37499999999998401, -20.99999999999999645, 3.666666666666654084 ) ) ;
#12889 = FACE_OUTER_BOUND ( 'NONE', #17124, .T. ) ;
#12890 = CARTESIAN_POINT ( 'NONE',  ( 5.034691417683177406, -19.47900456129164581, 2.515153566944927199 ) ) ;
#12891 = CARTESIAN_POINT ( 'NONE',  ( -9.621558582316795949, -22.99999999999999645, 3.550687472877652073 ) ) ;
#12892 = VERTEX_POINT ( 'NONE', #10461 ) ;
#12893 = CARTESIAN_POINT ( 'NONE',  ( 13.90394305879618386, 5.711624469205903942, 5.287712306078340418 ) ) ;
#12894 = CARTESIAN_POINT ( 'NONE',  ( 12.68288333306630378, -17.32689168014509207, 5.548858176248425700 ) ) ;
#12895 = CARTESIAN_POINT ( 'NONE',  ( -11.00000000000000000, -25.49999999999999645, 6.500000000000000000 ) ) ;
#12896 = EDGE_LOOP ( 'NONE', ( #9945, #8852, #7508, #17014 ) ) ;
#12897 = VERTEX_POINT ( 'NONE', #19884 ) ;
#12898 = DIRECTION ( 'NONE',  ( -0.000000000000000000, -0.000000000000000000, -1.000000000000000000 ) ) ;
#12899 = DIRECTION ( 'NONE',  ( 0.000000000000000000, 1.000000000000000000, 0.000000000000000000 ) ) ;
#12900 = LINE ( 'NONE', #12496, #3642 ) ;
#12901 = CYLINDRICAL_SURFACE ( 'NONE', #7662, 10.00000000000000000 ) ;
#12902 = CARTESIAN_POINT ( 'NONE',  ( 2.041623931606483033, -10.12028065167953272, 1.688226231982305370 ) ) ;
#12903 = DIRECTION ( 'NONE',  ( 0.000000000000000000, -1.000000000000000000, 0.000000000000000000 ) ) ;
#12904 = AXIS2_PLACEMENT_3D ( 'NONE', #5262, #13308, #3805 ) ;
#12905 = LINE ( 'NONE', #1731, #4752 ) ;
#12906 = ADVANCED_FACE ( 'NONE', ( #15052 ), #2494, .F. ) ;
#12907 = CARTESIAN_POINT ( 'NONE',  ( 5.999999999999999112, -7.500000000000047073, 8.999999999999998224 ) ) ;
#12908 = FACE_OUTER_BOUND ( 'NONE', #16915, .T. ) ;
#12909 = DIRECTION ( 'NONE',  ( 0.000000000000000000, 1.000000000000000000, -0.000000000000000000 ) ) ;
#12910 = CARTESIAN_POINT ( 'NONE',  ( -1.126276606324276619, -9.114917468222230923, 2.372643865078341019 ) ) ;
#12911 = VECTOR ( 'NONE', #2673, 1000.000000000000000 ) ;
#12912 = CARTESIAN_POINT ( 'NONE',  ( -12.63118877378512828, -19.18746692385052555, 4.758813856674282583 ) ) ;
#12913 = CARTESIAN_POINT ( 'NONE',  ( -5.027808582316795949, -22.97900456129165647, 3.964901035250747885 ) ) ;
#12914 = CARTESIAN_POINT ( 'NONE',  ( -5.597191417683179182, -22.77556120703057729, 5.229004561291655584 ) ) ;
#12915 = ORIENTED_EDGE ( 'NONE', *, *, #15424, .T. ) ;
#12916 = CARTESIAN_POINT ( 'NONE',  ( 13.84051394328565365, 4.008454135954084840, 5.243107695145536873 ) ) ;
#12917 = DIRECTION ( 'NONE',  ( 1.000000000000000000, 0.000000000000000000, 0.000000000000000000 ) ) ;
#12918 = ORIENTED_EDGE ( 'NONE', *, *, #19128, .F. ) ;
#12919 = EDGE_CURVE ( 'NONE', #19171, #6959, #5754, .T. ) ;
#12920 = ORIENTED_EDGE ( 'NONE', *, *, #8864, .T. ) ;
#12921 = LINE ( 'NONE', #581, #14064 ) ;
#12922 = EDGE_LOOP ( 'NONE', ( #13177, #1790, #1025, #3538 ) ) ;
#12923 = LINE ( 'NONE', #14596, #11428 ) ;
#12924 = VECTOR ( 'NONE', #17157, 1000.000000000000000 ) ;
#12925 = VERTEX_POINT ( 'NONE', #8889 ) ;
#12926 = CARTESIAN_POINT ( 'NONE',  ( 10.56594141768317741, -23.20159541128344927, 2.226721677130534705 ) ) ;
#12927 = DIRECTION ( 'NONE',  ( 1.000000000000000000, 0.000000000000000000, 0.000000000000000000 ) ) ;
#12928 = CARTESIAN_POINT ( 'NONE',  ( 0.000000000000000000, -9.114917468222230923, 2.372643865078340575 ) ) ;
#12929 = DIRECTION ( 'NONE',  ( 0.000000000000000000, 0.000000000000000000, -1.000000000000000000 ) ) ;
#12930 = CARTESIAN_POINT ( 'NONE',  ( -11.96530858231679417, -20.22900456129164937, 4.174186261275266929 ) ) ;
#12931 = EDGE_CURVE ( 'NONE', #11608, #12110, #14615, .T. ) ;
#12932 = LINE ( 'NONE', #19335, #2279 ) ;
#12933 = CARTESIAN_POINT ( 'NONE',  ( 11.69094141768317563, -23.27327832286946219, 4.701595411283453707 ) ) ;
#12934 = DIRECTION ( 'NONE',  ( -1.000000000000000000, 0.000000000000000000, -0.000000000000000000 ) ) ;
#12935 = CARTESIAN_POINT ( 'NONE',  ( -10.84719141768317741, -21.53509896474923835, 2.520995438708346192 ) ) ;
#12936 = ORIENTED_EDGE ( 'NONE', *, *, #18887, .F. ) ;
#12937 = CARTESIAN_POINT ( 'NONE',  ( 10.46530858231679595, -19.47900456129164937, 4.484846433055089676 ) ) ;
#12938 = ADVANCED_FACE ( 'NONE', ( #16830 ), #18994, .F. ) ;
#12939 = CARTESIAN_POINT ( 'NONE',  ( 13.10756170493883310, 4.119366099410778581, 6.001761809183453700 ) ) ;
#12940 = CARTESIAN_POINT ( 'NONE',  ( -12.64323021897839006, -19.32937394158751943, 5.504219675487169283 ) ) ;
#12941 = ORIENTED_EDGE ( 'NONE', *, *, #12607, .F. ) ;
#12942 = EDGE_CURVE ( 'NONE', #5157, #7736, #19038, .T. ) ;
#12943 = DIRECTION ( 'NONE',  ( 1.000000000000000000, -0.000000000000000000, 0.000000000000000000 ) ) ;
#12944 = CARTESIAN_POINT ( 'NONE',  ( 13.12509927631103501, 5.009931486494128450, 3.999999999999983125 ) ) ;
#12945 = APPLICATION_CONTEXT ( 'automotive_design' ) ;
#12946 = ORIENTED_EDGE ( 'NONE', *, *, #16692, .T. ) ;
#12947 = DIRECTION ( 'NONE',  ( 0.000000000000000000, 0.000000000000000000, 1.000000000000000000 ) ) ;
#12948 = VERTEX_POINT ( 'NONE', #4588 ) ;
#12949 = EDGE_CURVE ( 'NONE', #20223, #2296, #12743, .T. ) ;
#12950 = CARTESIAN_POINT ( 'NONE',  ( -15.87779268661489773, 11.64110105645932691, 10.00000000000000000 ) ) ;
#12951 = ORIENTED_EDGE ( 'NONE', *, *, #11165, .F. ) ;
#12952 = CARTESIAN_POINT ( 'NONE',  ( -12.24655858231679595, -21.94931252712234127, 6.000000000000001776 ) ) ;
#12953 = LINE ( 'NONE', #7847, #20317 ) ;
#12954 = MECHANICAL_DESIGN_GEOMETRIC_PRESENTATION_REPRESENTATION (  '', ( #7955 ), #4959 ) ;
#12955 = LINE ( 'NONE', #11287, #16812 ) ;
#12956 = CARTESIAN_POINT ( 'NONE',  ( 1.711347482507859397, -9.865394108634699677, 1.622766275858107621 ) ) ;
#12957 = VECTOR ( 'NONE', #20276, 1000.000000000000000 ) ;
#12958 = ADVANCED_FACE ( 'NONE', ( #4897 ), #9713, .T. ) ;
#12959 = CARTESIAN_POINT ( 'NONE',  ( 13.05696142222617695, 1.564051822406025583, 5.955108176248398166 ) ) ;
#12960 = CARTESIAN_POINT ( 'NONE',  ( 1.937849085826861328, 11.64110105645932691, 10.00000000000000000 ) ) ;
#12961 = CARTESIAN_POINT ( 'NONE',  ( -13.84501469867711698, 4.235742283194553259, 4.791666666666684726 ) ) ;
#12962 = CARTESIAN_POINT ( 'NONE',  ( 8.309058582316795949, -23.80360840875935935, 1.768074502826626260 ) ) ;
#12963 = CARTESIAN_POINT ( 'NONE',  ( -13.13728495444130751, 4.870390199291127153, 6.548325014280736767 ) ) ;
#12964 = CARTESIAN_POINT ( 'NONE',  ( 26.69203811574920238, 10.00000000000000000, 0.000000000000000000 ) ) ;
#12965 = FACE_OUTER_BOUND ( 'NONE', #12275, .T. ) ;
#12966 = VECTOR ( 'NONE', #16918, 1000.000000000000000 ) ;
#12967 = CARTESIAN_POINT ( 'NONE',  ( 3.974842109207560537, -21.92432777746334693, 4.506404853634142782 ) ) ;
#12968 = CARTESIAN_POINT ( 'NONE',  ( -9.628441417683177406, -20.24999999999999289, 3.550687472877664952 ) ) ;
#12969 = VECTOR ( 'NONE', #18385, 1000.000000000000000 ) ;
#12970 = ORIENTED_EDGE ( 'NONE', *, *, #19370, .T. ) ;
#12971 = ORIENTED_EDGE ( 'NONE', *, *, #6332, .F. ) ;
#12972 = CARTESIAN_POINT ( 'NONE',  ( 13.83411111208379474, 3.685111160228107252, 5.236156213382356484 ) ) ;
#12973 = DIRECTION ( 'NONE',  ( 0.000000000000000000, 1.000000000000000000, 0.000000000000000000 ) ) ;
#12974 = DIRECTION ( 'NONE',  ( 0.000000000000000000, 0.000000000000000000, -1.000000000000000000 ) ) ;
#12975 = EDGE_LOOP ( 'NONE', ( #16891, #9272, #7962, #1563 ) ) ;
#12976 = EDGE_CURVE ( 'NONE', #193, #14057, #1767, .T. ) ;
#12977 = ORIENTED_EDGE ( 'NONE', *, *, #8729, .F. ) ;
#12978 = DIRECTION ( 'NONE',  ( -0.000000000000000000, 0.000000000000000000, -1.000000000000000000 ) ) ;
#12979 = DIRECTION ( 'NONE',  ( -1.000000000000000000, 0.000000000000000000, 0.000000000000000000 ) ) ;
#12980 = DIRECTION ( 'NONE',  ( 0.000000000000000000, 0.000000000000000000, 1.000000000000000000 ) ) ;
#12981 = VECTOR ( 'NONE', #6840, 1000.000000000000000 ) ;
#12982 = DIRECTION ( 'NONE',  ( 1.000000000000000000, 0.000000000000000000, 0.000000000000000000 ) ) ;
#12983 = CARTESIAN_POINT ( 'NONE',  ( 0.000000000000000000, -8.364917468222230923, 1.622643865078341241 ) ) ;
#12984 = ADVANCED_FACE ( 'NONE', ( #9916 ), #8250, .T. ) ;
#12985 = VECTOR ( 'NONE', #2206, 1000.000000000000000 ) ;
#12986 = EDGE_CURVE ( 'NONE', #12435, #3029, #10225, .T. ) ;
#12987 = PLANE ( 'NONE',  #18758 ) ;
#12988 = CARTESIAN_POINT ( 'NONE',  ( -13.10624331898488037, 4.052787608736739600, 6.006964772046813117 ) ) ;
#12989 = FILL_AREA_STYLE_COLOUR ( '', #19466 ) ;
#12990 = DIRECTION ( 'NONE',  ( 0.000000000000000000, 1.000000000000000000, 0.000000000000000000 ) ) ;
#12991 = CARTESIAN_POINT ( 'NONE',  ( 12.64751377014909828, -19.11305460747000495, 5.510446717915143289 ) ) ;
#12992 = CARTESIAN_POINT ( 'NONE',  ( -0.5631383031621635116, -9.864917468222230923, 2.372643865078341019 ) ) ;
#12993 = ORIENTED_EDGE ( 'NONE', *, *, #16161, .T. ) ;
#12994 = CARTESIAN_POINT ( 'NONE',  ( -13.85528666703740619, 4.004476685417483139, 5.993048563355776182 ) ) ;
#12995 = CARTESIAN_POINT ( 'NONE',  ( 0.000000000000000000, 4.999999999999999112, 0.000000000000000000 ) ) ;
#12996 = CARTESIAN_POINT ( 'NONE',  ( 6.347191417683176518, -20.91377862118959285, 1.020995438708345082 ) ) ;
#12997 = CARTESIAN_POINT ( 'NONE',  ( -4.934058582316795061, -22.67126532539354855, 4.242948236979545484 ) ) ;
#12998 = VERTEX_POINT ( 'NONE', #14517 ) ;
#12999 = CARTESIAN_POINT ( 'NONE',  ( 13.60059015675642513, -9.607697083824668027, 6.450359435862663027 ) ) ;
#13000 = CARTESIAN_POINT ( 'NONE',  ( 13.10012427866737639, 3.743776072700027324, 6.001983176248468332 ) ) ;
#13001 = VECTOR ( 'NONE', #14789, 1000.000000000000000 ) ;
#13002 = AXIS2_PLACEMENT_3D ( 'NONE', #13756, #7494, #4039 ) ;
#13003 = DIRECTION ( 'NONE',  ( 1.000000000000000000, 0.000000000000000000, -0.000000000000000000 ) ) ;
#13004 = VERTEX_POINT ( 'NONE', #8460 ) ;
#13005 = EDGE_CURVE ( 'NONE', #1137, #7916, #5208, .T. ) ;
#13006 = VECTOR ( 'NONE', #13562, 1000.000000000000000 ) ;
#13007 = ORIENTED_EDGE ( 'NONE', *, *, #1682, .T. ) ;
#13008 = LINE ( 'NONE', #4853, #1758 ) ;
#13009 = CARTESIAN_POINT ( 'NONE',  ( -13.37327929115833491, -20.24999999560066399, 3.449077790995343840 ) ) ;
#13010 = DIRECTION ( 'NONE',  ( 4.625929269271477434E-15, 1.000000000000000000, 0.000000000000000000 ) ) ;
#13011 = DIRECTION ( 'NONE',  ( 0.000000000000000000, 0.000000000000000000, -1.000000000000000000 ) ) ;
#13012 = CARTESIAN_POINT ( 'NONE',  ( 1.859341899742023463, -9.902476528685241419, 1.632289782122827271 ) ) ;
#13013 = CARTESIAN_POINT ( 'NONE',  ( -2.499999999999998668, -19.50000000000000000, 1.000000000000000000 ) ) ;
#13014 = LINE ( 'NONE', #19107, #1416 ) ;
#13015 = LINE ( 'NONE', #9674, #1345 ) ;
#13016 = CIRCLE ( 'NONE', #3658, 10.00000000000000000 ) ;
#13017 = CARTESIAN_POINT ( 'NONE',  ( 13.49999999999998401, -18.49999999999999645, 4.000000000000000000 ) ) ;
#13018 = CARTESIAN_POINT ( 'NONE',  ( -0.1250000000000035805, 9.000000000000000000, 1.000000000000000000 ) ) ;
#13019 = CARTESIAN_POINT ( 'NONE',  ( -12.80487140268466817, -20.58484656434375637, 3.526619154972564285 ) ) ;
#13020 = ORIENTED_EDGE ( 'NONE', *, *, #7199, .T. ) ;
#13021 = CARTESIAN_POINT ( 'NONE',  ( -12.72590726430969532, -14.40418315237199742, 4.861678440007700885 ) ) ;
#13022 = CARTESIAN_POINT ( 'NONE',  ( -4.934058582316795061, -22.67126532539354855, 4.242948236979545484 ) ) ;
#13023 = VECTOR ( 'NONE', #20190, 1000.000000000000000 ) ;
#13024 = CARTESIAN_POINT ( 'NONE',  ( -6.159691417683176518, -22.67418626127524917, 1.729004561291651809 ) ) ;
#13025 = ORIENTED_EDGE ( 'NONE', *, *, #11102, .F. ) ;
#13026 = CARTESIAN_POINT ( 'NONE',  ( 13.84476264919594612, 4.223013784394161974, 5.079233071712400793 ) ) ;
#13027 = CARTESIAN_POINT ( 'NONE',  ( 9.555650798910054533, 4.999999999999999112, 1.000000000000000000 ) ) ;
#13028 = VERTEX_POINT ( 'NONE', #18182 ) ;
#13029 = ORIENTED_EDGE ( 'NONE', *, *, #15607, .F. ) ;
#13030 = ADVANCED_FACE ( 'NONE', ( #194 ), #3438, .T. ) ;
#13031 = LINE ( 'NONE', #4877, #17403 ) ;
#13032 = ORIENTED_EDGE ( 'NONE', *, *, #8984, .T. ) ;
#13033 = CARTESIAN_POINT ( 'NONE',  ( 23.31633994409548549, 10.00000000000000000, 0.000000000000000000 ) ) ;
#13034 = ADVANCED_FACE ( 'NONE', ( #13358 ), #16499, .T. ) ;
#13035 = AXIS2_PLACEMENT_3D ( 'NONE', #125, #6713, #6510 ) ;
#13036 = ORIENTED_EDGE ( 'NONE', *, *, #4649, .F. ) ;
#13037 = CARTESIAN_POINT ( 'NONE',  ( -13.81494360078803396, 16.00000000000000000, 1.000000000000000000 ) ) ;
#13038 = CARTESIAN_POINT ( 'NONE',  ( 5.000000000000000000, -7.500000000000000000, 1.000000000000000000 ) ) ;
#13039 = AXIS2_PLACEMENT_3D ( 'NONE', #8184, #6817, #4931 ) ;
#13040 = CARTESIAN_POINT ( 'NONE',  ( -1.668644041176298387, -9.864915931696323526, 2.372643470467795890 ) ) ;
#13041 = CARTESIAN_POINT ( 'NONE',  ( 2.109407804498405703, -9.207748739546751438, 2.396484790045401603 ) ) ;
#13042 = CARTESIAN_POINT ( 'NONE',  ( -11.40280858231679595, -22.77556120703056308, 1.770995438708340197 ) ) ;
#13043 = SURFACE_STYLE_FILL_AREA ( #283 ) ;
#13044 = CARTESIAN_POINT ( 'NONE',  ( 6.815941417683176518, -20.79840458871654363, 4.773278322869464851 ) ) ;
#13045 = CARTESIAN_POINT ( 'NONE',  ( -7.499999999999999112, -18.49999999999999645, 6.500000000000000888 ) ) ;
#13046 = CARTESIAN_POINT ( 'NONE',  ( -10.56594141768317741, -22.67126532539353789, 2.757051763020445634 ) ) ;
#13047 = EDGE_LOOP ( 'NONE', ( #4775, #2765, #4806, #4063 ) ) ;
#13048 = CARTESIAN_POINT ( 'NONE',  ( 9.902808582316795949, -23.08622137881038938, 1.020995438708339309 ) ) ;
#13049 = CARTESIAN_POINT ( 'NONE',  ( 12.64571531779736979, -19.20387645123237164, 5.508493592915143289 ) ) ;
#13050 = CARTESIAN_POINT ( 'NONE',  ( -12.62500016093973620, -20.24999187254239175, 4.532396751752561848 ) ) ;
#13051 = ORIENTED_EDGE ( 'NONE', *, *, #6918, .F. ) ;
#13052 = VECTOR ( 'NONE', #16883, 1000.000000000000000 ) ;
#13053 = VECTOR ( 'NONE', #10716, 1000.000000000000000 ) ;
#13054 = DIRECTION ( 'NONE',  ( 0.000000000000000000, -0.000000000000000000, 1.000000000000000000 ) ) ;
#13055 = CARTESIAN_POINT ( 'NONE',  ( -24.12918902992234393, 10.00000000000000000, 1.000000000000000000 ) ) ;
#13056 = VECTOR ( 'NONE', #7364, 1000.000000000000000 ) ;
#13057 = VERTEX_POINT ( 'NONE', #5001 ) ;
#13058 = ORIENTED_EDGE ( 'NONE', *, *, #1948, .T. ) ;
#13059 = EDGE_CURVE ( 'NONE', #7068, #1942, #17869, .T. ) ;
#13060 = CARTESIAN_POINT ( 'NONE',  ( 26.69203811574920238, 11.64110105645932691, 10.00000000000000000 ) ) ;
#13061 = ORIENTED_EDGE ( 'NONE', *, *, #16926, .F. ) ;
#13062 = CARTESIAN_POINT ( 'NONE',  ( -11.40280858231679595, -23.08622137881038938, 1.020995438708339309 ) ) ;
#13063 = CARTESIAN_POINT ( 'NONE',  ( 13.06655316810189227, 2.048434989138931961, 5.965524842914772030 ) ) ;
#13064 = EDGE_CURVE ( 'NONE', #2576, #7246, #14729, .T. ) ;
#13065 = CARTESIAN_POINT ( 'NONE',  ( -0.000000000000000000, 11.64110105645932691, 0.000000000000000000 ) ) ;
#13066 = EDGE_CURVE ( 'NONE', #10351, #8244, #10958, .T. ) ;
#13067 = AXIS2_PLACEMENT_3D ( 'NONE', #19497, #16239, #13094 ) ;
#13068 = CARTESIAN_POINT ( 'NONE',  ( 12.95145221759166354, -3.764163011652346569, 5.840524842913703552 ) ) ;
#13069 = FACE_OUTER_BOUND ( 'NONE', #12887, .T. ) ;
#13070 = CARTESIAN_POINT ( 'NONE',  ( -13.37500000000002132, -20.24999999999450040, 3.833333333368183382 ) ) ;
#13071 = CARTESIAN_POINT ( 'NONE',  ( 12.05905858231679595, -20.19639159124062999, 5.231925497173373074 ) ) ;
#13072 = CARTESIAN_POINT ( 'NONE',  ( -12.62499999999998579, -20.24999999999999289, 3.146526952850934755 ) ) ;
#13073 = CARTESIAN_POINT ( 'NONE',  ( -6.152808582316795949, -20.91377862118960351, 5.979004561291660913 ) ) ;
#13074 = DIRECTION ( 'NONE',  ( 0.000000000000000000, -0.000000000000000000, -1.000000000000000000 ) ) ;
#13075 = DIRECTION ( 'NONE',  ( 1.000000000000000000, 0.000000000000000000, 0.000000000000000000 ) ) ;
#13076 = CARTESIAN_POINT ( 'NONE',  ( 8.402808582316797725, -22.46490103525074034, 2.520995438708341307 ) ) ;
#13077 = CARTESIAN_POINT ( 'NONE',  ( -7.753441417683176518, -21.94931252712233061, 1.749999999999998446 ) ) ;
#13078 = ORIENTED_EDGE ( 'NONE', *, *, #2847, .F. ) ;
#13079 = ORIENTED_EDGE ( 'NONE', *, *, #7565, .T. ) ;
#13080 = CARTESIAN_POINT ( 'NONE',  ( 13.38238173943565990, -19.87722215849730034, 5.285856107751903288 ) ) ;
#13081 = LINE ( 'NONE', #14854, #9438 ) ;
#13082 = SURFACE_SIDE_STYLE ('',( #3564 ) ) ;
#13083 = VERTEX_POINT ( 'NONE', #6683 ) ;
#13084 = VECTOR ( 'NONE', #7498, 1000.000000000000000 ) ;
#13085 = EDGE_CURVE ( 'NONE', #5367, #5490, #9816, .T. ) ;
#13086 = ORIENTED_EDGE ( 'NONE', *, *, #10682, .F. ) ;
#13087 = CARTESIAN_POINT ( 'NONE',  ( 4.000000000000000000, -8.500000000000000000, 1.000000000000000000 ) ) ;
#13088 = DIRECTION ( 'NONE',  ( 1.000000000000000000, -0.000000000000000000, 0.000000000000000000 ) ) ;
#13089 = CARTESIAN_POINT ( 'NONE',  ( 13.37499979530394967, -20.25001033714808329, 4.458488164327452097 ) ) ;
#13090 = LINE ( 'NONE', #14163, #15864 ) ;
#13091 = LINE ( 'NONE', #13288, #5719 ) ;
#13092 = CARTESIAN_POINT ( 'NONE',  ( -12.64571531779736979, -19.20387645123237164, 5.508493592915143289 ) ) ;
#13093 = CARTESIAN_POINT ( 'NONE',  ( 4.934058582316793284, -23.20159541128345992, 4.773278322869455970 ) ) ;
#13094 = DIRECTION ( 'NONE',  ( -0.000000000000000000, 0.000000000000000000, -1.000000000000000000 ) ) ;
#13095 = CARTESIAN_POINT ( 'NONE',  ( 13.10252221513633941, 3.864871864382954048, 6.004587342915129966 ) ) ;
#13096 = VECTOR ( 'NONE', #20671, 1000.000000000000000 ) ;
#13097 = CARTESIAN_POINT ( 'NONE',  ( -3.047379876266447685, -13.13734219723468755, 3.405682891496055742 ) ) ;
#13098 = ORIENTED_EDGE ( 'NONE', *, *, #9328, .F. ) ;
#13099 = CARTESIAN_POINT ( 'NONE',  ( -13.87215786865436762, 4.856472367046606564, 5.506273593909547515 ) ) ;
#13100 = DIRECTION ( 'NONE',  ( -1.000000000000000000, 0.000000000000000000, 0.000000000000000000 ) ) ;
#13101 = CARTESIAN_POINT ( 'NONE',  ( 9.909691417683179182, -21.32581373872474373, 5.270995438708348857 ) ) ;
#13102 = CARTESIAN_POINT ( 'NONE',  ( -10.65280858231679595, -21.53509896474924901, 4.479004561291659137 ) ) ;
#13103 = EDGE_LOOP ( 'NONE', ( #4364, #6211, #16122, #5517 ) ) ;
#13104 = CARTESIAN_POINT ( 'NONE',  ( 13.87824226375436965, 4.413734319597230282, 6.694665752684481497 ) ) ;
#13105 = CARTESIAN_POINT ( 'NONE',  ( 13.02818618459764188, 0.1109023222084986743, 5.923858176248589125 ) ) ;
#13106 = DIRECTION ( 'NONE',  ( -0.000000000000000000, 0.000000000000000000, -1.000000000000000000 ) ) ;
#13107 = VECTOR ( 'NONE', #8077, 1000.000000000000000 ) ;
#13108 = ORIENTED_EDGE ( 'NONE', *, *, #8347, .T. ) ;
#13109 = ADVANCED_FACE ( 'NONE', ( #5418 ), #8555, .T. ) ;
#13110 = ORIENTED_EDGE ( 'NONE', *, *, #15990, .T. ) ;
#13111 = EDGE_CURVE ( 'NONE', #14385, #9688, #1867, .T. ) ;
#13112 = LINE ( 'NONE', #17921, #17128 ) ;
#13113 = AXIS2_PLACEMENT_3D ( 'NONE', #18341, #15089, #13518 ) ;
#13114 = CARTESIAN_POINT ( 'NONE',  ( 0.000000000000000000, 4.999999999999999112, 0.000000000000000000 ) ) ;
#13115 = EDGE_CURVE ( 'NONE', #7202, #12948, #5110, .T. ) ;
#13116 = CARTESIAN_POINT ( 'NONE',  ( -9.000000000000000000, -9.999999999999992895, 1.000000000000000000 ) ) ;
#13117 = LINE ( 'NONE', #10086, #3654 ) ;
#13118 = CARTESIAN_POINT ( 'NONE',  ( 0.2815691515810352930, -9.114917468222230923, 1.622643865078524206 ) ) ;
#13119 = DIRECTION ( 'NONE',  ( -1.000000000000000000, 0.000000000000000000, 0.000000000000000000 ) ) ;
#13120 = LINE ( 'NONE', #16558, #8062 ) ;
#13121 = EDGE_CURVE ( 'NONE', #8657, #17919, #6882, .T. ) ;
#13122 = CARTESIAN_POINT ( 'NONE',  ( -14.49999999999998579, -24.47992105705875332, 12.00000000000000000 ) ) ;
#13123 = PLANE ( 'NONE',  #956 ) ;
#13124 = CARTESIAN_POINT ( 'NONE',  ( -8.215308582316792396, -23.77099543870833998, 2.825813738724734847 ) ) ;
#13125 = CARTESIAN_POINT ( 'NONE',  ( -3.211992482548209349, -9.366834950279640637, 2.629956289783360823 ) ) ;
#13126 = ORIENTED_EDGE ( 'NONE', *, *, #8695, .T. ) ;
#13127 = CARTESIAN_POINT ( 'NONE',  ( -13.08439876642066935, 3.699637704240349656, 5.251001356674258602 ) ) ;
#13128 = CARTESIAN_POINT ( 'NONE',  ( -10.27780858231679417, -20.27099543870833642, 2.724438792969431589 ) ) ;
#13129 = VECTOR ( 'NONE', #4808, 1000.000000000000000 ) ;
#13130 = CARTESIAN_POINT ( 'NONE',  ( -9.065941417683177406, -23.20159541128344927, 2.226721677130534705 ) ) ;
#13131 = ORIENTED_EDGE ( 'NONE', *, *, #19227, .F. ) ;
#13132 = CARTESIAN_POINT ( 'NONE',  ( 13.64827103573800571, -5.699812695207630675, 5.034333296717131034 ) ) ;
#13133 = CARTESIAN_POINT ( 'NONE',  ( 4.000698171653723101, 16.00000000000000000, 1.000000000000000000 ) ) ;
#13134 = VERTEX_POINT ( 'NONE', #13252 ) ;
#13135 = VERTEX_POINT ( 'NONE', #5308 ) ;
#13136 = DIRECTION ( 'NONE',  ( 0.000000000000000000, -1.000000000000000000, 0.000000000000000000 ) ) ;
#13137 = ORIENTED_EDGE ( 'NONE', *, *, #7884, .F. ) ;
#13138 = DIRECTION ( 'NONE',  ( 1.000000000000000000, 0.000000000000000000, 0.000000000000000000 ) ) ;
#13139 = VECTOR ( 'NONE', #10781, 1000.000000000000000 ) ;
#13140 = ORIENTED_EDGE ( 'NONE', *, *, #1990, .T. ) ;
#13141 = CARTESIAN_POINT ( 'NONE',  ( 4.378441417683176518, -23.74999999999999645, 3.449312527122335492 ) ) ;
#13142 = CARTESIAN_POINT ( 'NONE',  ( 25.54469207716615031, 4.999999999999999112, 1.000000000000000000 ) ) ;
#13143 = LINE ( 'NONE', #19541, #1303 ) ;
#13144 = DIRECTION ( 'NONE',  ( -0.000000000000000000, 1.304178812473495102E-15, 1.000000000000000000 ) ) ;
#13145 = FACE_OUTER_BOUND ( 'NONE', #15238, .T. ) ;
#13146 = EDGE_CURVE ( 'NONE', #6320, #3742, #10621, .T. ) ;
#13147 =( NAMED_UNIT ( * ) PLANE_ANGLE_UNIT ( ) SI_UNIT ( $, .RADIAN. ) );
#13148 = CARTESIAN_POINT ( 'NONE',  ( 11.59719141768317563, -22.77556120703057729, 5.229004561291655584 ) ) ;
#13149 = CARTESIAN_POINT ( 'NONE',  ( -15.11404127825609223, 0.000000000000000000, 1.000000000000000000 ) ) ;
#13150 = CARTESIAN_POINT ( 'NONE',  ( -10.09719141768317741, -22.46490103525075810, 4.479004561291653808 ) ) ;
#13151 = VERTEX_POINT ( 'NONE', #14616 ) ;
#13152 = CARTESIAN_POINT ( 'NONE',  ( 8.684058582316795949, -20.26807450282662160, 1.696391591240633101 ) ) ;
#13153 = CARTESIAN_POINT ( 'NONE',  ( 12.65650603190776025, -18.65894538865861563, 5.520212342915047365 ) ) ;
#13154 = CARTESIAN_POINT ( 'NONE',  ( -12.62499999999998224, -20.24999999999998934, 4.166666666666636765 ) ) ;
#13155 = ORIENTED_EDGE ( 'NONE', *, *, #7079, .F. ) ;
#13156 = CARTESIAN_POINT ( 'NONE',  ( 27.49999999999999645, -4.770489558936219510E-14, 1.000000000000000000 ) ) ;
#13157 = CARTESIAN_POINT ( 'NONE',  ( 0.000000000000000000, 16.00000000000000000, 1.000000000000000000 ) ) ;
#13158 = VERTEX_POINT ( 'NONE', #294 ) ;
#13159 = APPLICATION_PROTOCOL_DEFINITION ( 'draft international standard', 'automotive_design', 1998, #19780 ) ;
#13160 = ORIENTED_EDGE ( 'NONE', *, *, #19492, .F. ) ;
#13161 = DIRECTION ( 'NONE',  ( -1.000000000000000000, -5.782411586589356653E-16, 0.000000000000000000 ) ) ;
#13162 = EDGE_LOOP ( 'NONE', ( #6738, #8054, #11159, #12738 ) ) ;
#13163 = FACE_OUTER_BOUND ( 'NONE', #17915, .T. ) ;
#13164 = CARTESIAN_POINT ( 'NONE',  ( 13.12529397354238192, 5.014845663890295846, 4.791666666666685614 ) ) ;
#13165 = DIRECTION ( 'NONE',  ( -1.000000000000000000, 0.000000000000000000, 0.000000000000000000 ) ) ;
#13166 = CARTESIAN_POINT ( 'NONE',  ( 13.15498530132288479, 5.764257716805535559, 4.333333333333380999 ) ) ;
#13167 = CARTESIAN_POINT ( 'NONE',  ( -5.999999999999999112, -2.500000000000047518, 9.999999999999998224 ) ) ;
#13168 = CARTESIAN_POINT ( 'NONE',  ( -13.37499999999998224, -20.24999999999998934, 4.291666666666698937 ) ) ;
#13169 = CARTESIAN_POINT ( 'NONE',  ( 12.43405858231679595, -23.73192549717337130, 5.303608408759367343 ) ) ;
#13170 = CARTESIAN_POINT ( 'NONE',  ( -12.62499999999998224, -20.24999999999991829, 4.333333333333343695 ) ) ;
#13171 = CARTESIAN_POINT ( 'NONE',  ( -12.06594141768317741, -23.73192549717336064, 1.696391591240623331 ) ) ;
#13172 = ADVANCED_FACE ( 'NONE', ( #5737 ), #2270, .T. ) ;
#13173 = CARTESIAN_POINT ( 'NONE',  ( 0.000000000000000000, 4.999999999999999112, 0.000000000000000000 ) ) ;
#13174 = LINE ( 'NONE', #11604, #20116 ) ;
#13175 = CARTESIAN_POINT ( 'NONE',  ( 9.059058582316795949, -21.25705176302045274, 4.171265325393551215 ) ) ;
#13176 = CARTESIAN_POINT ( 'NONE',  ( -4.565941417683176518, -23.20159541128344927, 2.226721677130534705 ) ) ;
#13177 = ORIENTED_EDGE ( 'NONE', *, *, #7824, .F. ) ;
#13178 = VERTEX_POINT ( 'NONE', #712 ) ;
#13179 = ADVANCED_FACE ( 'NONE', ( #2478 ), #16910, .T. ) ;
#13180 = CARTESIAN_POINT ( 'NONE',  ( 13.39107665282975645, -19.43812903209671461, 5.476542851584349947 ) ) ;
#13181 = ADVANCED_FACE ( 'NONE', ( #1134 ), #8967, .T. ) ;
#13182 = CARTESIAN_POINT ( 'NONE',  ( 20.00000000000000000, 2.500000000000003997, 2.000000000000000000 ) ) ;
#13183 =( NAMED_UNIT ( * ) PLANE_ANGLE_UNIT ( ) SI_UNIT ( $, .RADIAN. ) );
#13184 = EDGE_LOOP ( 'NONE', ( #15243, #7511, #19793, #14908 ) ) ;
#13185 = CARTESIAN_POINT ( 'NONE',  ( -15.61404127825609223, 0.000000000000000000, 1.000000000000000000 ) ) ;
#13186 = DIRECTION ( 'NONE',  ( 0.000000000000000000, 0.000000000000000000, -1.000000000000000000 ) ) ;
#13187 = LINE ( 'NONE', #19583, #7307 ) ;
#13188 = CARTESIAN_POINT ( 'NONE',  ( 13.80667376788930056, 1.549525278393783179, 5.940263032956496048 ) ) ;
#13189 = FACE_BOUND ( 'NONE', #2664, .T. ) ;
#13190 = CARTESIAN_POINT ( 'NONE',  ( 1.548630333695928396, -9.114917468222230923, 2.372643865078341019 ) ) ;
#13191 = LINE ( 'NONE', #16630, #11384 ) ;
#13192 = CARTESIAN_POINT ( 'NONE',  ( -12.67794853492974561, -16.82609898603114118, 4.809595106674325216 ) ) ;
#13193 = CARTESIAN_POINT ( 'NONE',  ( 8.965308582316794173, -20.22900456129164937, 4.174186261275266929 ) ) ;
#13194 = DIRECTION ( 'NONE',  ( -0.000000000000000000, -0.000000000000000000, -1.000000000000000000 ) ) ;
#13195 = CARTESIAN_POINT ( 'NONE',  ( 12.63943061533661982, -19.52125392549825733, 5.470334935344855154 ) ) ;
#13196 = EDGE_CURVE ( 'NONE', #7246, #6003, #3599, .T. ) ;
#13197 = CARTESIAN_POINT ( 'NONE',  ( -2.367358971471363649, -9.400572650371021410, 2.446005822389718087 ) ) ;
#13198 = CARTESIAN_POINT ( 'NONE',  ( 10.18405858231679595, -21.32873467460644079, 2.757051763020455404 ) ) ;
#13199 = CARTESIAN_POINT ( 'NONE',  ( 11.78469141768317563, -23.77099543870834353, 4.174186261275252718 ) ) ;
#13200 = CARTESIAN_POINT ( 'NONE',  ( -5.777808582316795949, -21.02099543870833998, 3.035098964749253003 ) ) ;
#13201 = ORIENTED_EDGE ( 'NONE', *, *, #4151, .F. ) ;
#13202 = CARTESIAN_POINT ( 'NONE',  ( 12.62499999999998401, -20.99999999999999645, 3.666666666666654084 ) ) ;
#13203 = CARTESIAN_POINT ( 'NONE',  ( 12.64931222250080545, -19.02223276370786209, 5.512399842915133519 ) ) ;
#13204 = CARTESIAN_POINT ( 'NONE',  ( -13.84667963294518778, 4.277765388965502957, 4.000000000000000888 ) ) ;
#13205 = ORIENTED_EDGE ( 'NONE', *, *, #13695, .F. ) ;
#13206 = ORIENTED_EDGE ( 'NONE', *, *, #11102, .T. ) ;
#13207 = CARTESIAN_POINT ( 'NONE',  ( 2.499999999999999112, -24.49999999999999289, 1.000000000000000000 ) ) ;
#13208 = VECTOR ( 'NONE', #5794, 1000.000000000000000 ) ;
#13209 = DIRECTION ( 'NONE',  ( 0.000000000000000000, 0.000000000000000000, 1.000000000000000000 ) ) ;
#13210 = LINE ( 'NONE', #663, #9638 ) ;
#13211 = CARTESIAN_POINT ( 'NONE',  ( 25.37918902992234393, 10.00000000000000000, 1.000000000000000000 ) ) ;
#13212 = CARTESIAN_POINT ( 'NONE',  ( 2.057814715640970515, -10.20705538578787852, 1.710511717200805304 ) ) ;
#13213 = DIRECTION ( 'NONE',  ( -1.000000000000000000, 0.000000000000000000, 0.000000000000000000 ) ) ;
#13214 = CARTESIAN_POINT ( 'NONE',  ( -14.49999999999999645, -21.00000000000000355, 4.000000000000000000 ) ) ;
#13215 = CARTESIAN_POINT ( 'NONE',  ( 12.72644768880819477, -20.50652430979270946, 3.537312097732761895 ) ) ;
#13216 = CARTESIAN_POINT ( 'NONE',  ( -2.367358971471363649, -9.400572650371021410, 2.446005822389718087 ) ) ;
#13217 = CARTESIAN_POINT ( 'NONE',  ( -6.527808582316794173, -23.72900456129165647, 4.275561207030568411 ) ) ;
#13218 = EDGE_CURVE ( 'NONE', #5898, #20661, #18394, .T. ) ;
#13219 = CARTESIAN_POINT ( 'NONE',  ( -3.951988298270009636, -13.15210598010094323, 2.852089508627633219 ) ) ;
#13220 = ORIENTED_EDGE ( 'NONE', *, *, #3410, .F. ) ;
#13221 = VECTOR ( 'NONE', #19858, 1000.000000000000000 ) ;
#13222 = CARTESIAN_POINT ( 'NONE',  ( -12.67794853492974561, -16.82609898603114118, 4.809595106674325216 ) ) ;
#13223 = CARTESIAN_POINT ( 'NONE',  ( -7.934058582316792396, -23.20159541128345992, 4.773278322869455970 ) ) ;
#13224 = CARTESIAN_POINT ( 'NONE',  ( -7.472191417683176518, -23.72900456129165292, 2.724438792969417822 ) ) ;
#13225 = ORIENTED_EDGE ( 'NONE', *, *, #7013, .F. ) ;
#13226 = CARTESIAN_POINT ( 'NONE',  ( 13.68663801924254741, -3.762280028282741551, 5.075999963380942503 ) ) ;
#13227 = DIRECTION ( 'NONE',  ( -1.000000000000000000, -0.000000000000000000, 0.000000000000000000 ) ) ;
#13228 = VERTEX_POINT ( 'NONE', #19867 ) ;
#13229 = VERTEX_POINT ( 'NONE', #13875 ) ;
#13230 = CARTESIAN_POINT ( 'NONE',  ( 11.00000000000000000, -25.49999999999999645, 6.500000000000000000 ) ) ;
#13231 = ORIENTED_EDGE ( 'NONE', *, *, #14598, .F. ) ;
#13232 = CARTESIAN_POINT ( 'NONE',  ( -13.39170256340046095, -19.40652054827866380, 5.481861153867630065 ) ) ;
#13233 =( BOUNDED_CURVE ( )  B_SPLINE_CURVE ( 3, ( #7963, #20, #6408, #12773 ),
 .UNSPECIFIED., .F., .F. ) 
 B_SPLINE_CURVE_WITH_KNOTS ( ( 4, 4 ),
 ( 4.712388980384689674, 5.163415792180952479 ),
 .UNSPECIFIED. ) 
 CURVE ( )  GEOMETRIC_REPRESENTATION_ITEM ( )  RATIONAL_B_SPLINE_CURVE ( ( 1.000000000000000000, 0.9831196229872640746, 0.9831196229872640746, 1.000000000000000000 ) ) 
 REPRESENTATION_ITEM ( '' )  );
#13234 = ORIENTED_EDGE ( 'NONE', *, *, #18702, .T. ) ;
#13235 = CARTESIAN_POINT ( 'NONE',  ( 4.659691417683178294, -22.67418626127524917, 1.729004561291651587 ) ) ;
#13236 = CARTESIAN_POINT ( 'NONE',  ( -2.187849085826861550, 0.000000000000000000, 1.000000000000000000 ) ) ;
#13237 = LINE ( 'NONE', #13344, #6974 ) ;
#13238 = LINE ( 'NONE', #11574, #9656 ) ;
#13239 = CARTESIAN_POINT ( 'NONE',  ( -5.777808582316794173, -20.27099543870833642, 2.724438792969431589 ) ) ;
#13240 = EDGE_CURVE ( 'NONE', #16093, #18054, #12205, .T. ) ;
#13241 = CARTESIAN_POINT ( 'NONE',  ( 15.00000000000001599, -18.49999999999999645, 1.000000000000000000 ) ) ;
#13242 = EDGE_CURVE ( 'NONE', #13516, #14875, #912, .T. ) ;
#13243 = CARTESIAN_POINT ( 'NONE',  ( 11.12844141768317741, -20.24999999999999289, 3.550687472877664952 ) ) ;
#13244 = CARTESIAN_POINT ( 'NONE',  ( 10.05565079891005631, 0.000000000000000000, 0.000000000000000000 ) ) ;
#13245 = CARTESIAN_POINT ( 'NONE',  ( -5.690941417683177406, -22.74294823697955081, 4.171265325393542334 ) ) ;
#13246 = CARTESIAN_POINT ( 'NONE',  ( -9.715308582316795949, -24.52099543870834708, 2.515153566944913432 ) ) ;
#13247 = ORIENTED_EDGE ( 'NONE', *, *, #14763, .F. ) ;
#13248 = CARTESIAN_POINT ( 'NONE',  ( 12.66849571425264287, -18.05346643024382303, 5.533233176248494978 ) ) ;
#13249 = CARTESIAN_POINT ( 'NONE',  ( -12.62499979224180180, -20.25001049178813162, 4.458178821399696012 ) ) ;
#13250 = VERTEX_POINT ( 'NONE', #2380 ) ;
#13251 = AXIS2_PLACEMENT_3D ( 'NONE', #14983, #3700, #3904 ) ;
#13252 = CARTESIAN_POINT ( 'NONE',  ( 4.247260319564023945, 9.000000000000001776, 0.000000000000000000 ) ) ;
#13253 = CARTESIAN_POINT ( 'NONE',  ( -24.87918902992234393, 0.000000000000000000, 1.000000000000000000 ) ) ;
#13254 = ORIENTED_EDGE ( 'NONE', *, *, #3339, .F. ) ;
#13255 = PRODUCT_CONTEXT ( 'NONE', #20183, 'mechanical' ) ;
#13256 = ORIENTED_EDGE ( 'NONE', *, *, #7858, .T. ) ;
#13257 = EDGE_CURVE ( 'NONE', #4699, #11113, #10332, .T. ) ;
#13258 = CARTESIAN_POINT ( 'NONE',  ( 2.579281110863027582, -9.822567596814183233, 2.554382554832406615 ) ) ;
#13259 = VERTEX_POINT ( 'NONE', #11996 ) ;
#13260 = LINE ( 'NONE', #2083, #7638 ) ;
#13261 = CARTESIAN_POINT ( 'NONE',  ( 12.91308523408712183, -5.701695678577235249, 5.798858176249892082 ) ) ;
#13262 = CARTESIAN_POINT ( 'NONE',  ( 1.513434189748285696, -9.114917468222230923, 2.372643865078341019 ) ) ;
#13263 = LINE ( 'NONE', #10032, #4792 ) ;
#13264 = CARTESIAN_POINT ( 'NONE',  ( 12.64387510712649565, -19.29680709011273976, 5.506486987317513737 ) ) ;
#13265 = DIRECTION ( 'NONE',  ( -0.000000000000000000, -0.000000000000000000, -1.000000000000000000 ) ) ;
#13266 = CARTESIAN_POINT ( 'NONE',  ( 8.121558582316795949, -24.50000000000000000, 3.550687472877651629 ) ) ;
#13267 = CARTESIAN_POINT ( 'NONE',  ( -12.62515553039088090, -20.24214571525854467, 4.629702272822510345 ) ) ;
#13268 = CARTESIAN_POINT ( 'NONE',  ( -12.34719141768317741, -20.91377862118959285, 1.020995438708345082 ) ) ;
#13269 = DIRECTION ( 'NONE',  ( -0.000000000000000000, 0.000000000000000000, -1.000000000000000000 ) ) ;
#13270 = DIRECTION ( 'NONE',  ( -0.000000000000000000, 0.000000000000000000, -1.000000000000000000 ) ) ;
#13271 = CARTESIAN_POINT ( 'NONE',  ( 7.746558582316795949, -21.94931252712234127, 4.499999999999999112 ) ) ;
#13272 = PLANE ( 'NONE',  #1974 ) ;
#13273 = VERTEX_POINT ( 'NONE', #11890 ) ;
#13274 = ORIENTED_EDGE ( 'NONE', *, *, #7939, .F. ) ;
#13275 = CARTESIAN_POINT ( 'NONE',  ( 13.87470602645761986, 4.985154336109792972, 4.583333333333296622 ) ) ;
#13276 = CARTESIAN_POINT ( 'NONE',  ( -20.49999999999998224, -21.99999999999999645, 11.00000000000000178 ) ) ;
#13277 =( LENGTH_UNIT ( ) NAMED_UNIT ( * ) SI_UNIT ( .MILLI., .METRE. ) );
#13278 = VERTEX_POINT ( 'NONE', #18284 ) ;
#13279 = CARTESIAN_POINT ( 'NONE',  ( 4.247260319564023945, 4.999999999999999112, 1.000000000000000000 ) ) ;
#13280 = CARTESIAN_POINT ( 'NONE',  ( 0.000000000000000000, 10.00000000000000000, 1.000000000000000000 ) ) ;
#13281 = AXIS2_PLACEMENT_3D ( 'NONE', #3637, #14925, #16296 ) ;
#13282 = LINE ( 'NONE', #10259, #5631 ) ;
#13283 = EDGE_CURVE ( 'NONE', #4928, #19894, #8870, .T. ) ;
#13284 = CARTESIAN_POINT ( 'NONE',  ( 13.85163507668220539, 3.820071372449974412, 5.989091157956555556 ) ) ;
#13285 = AXIS2_PLACEMENT_3D ( 'NONE', #7493, #12394, #12287 ) ;
#13286 = DIRECTION ( 'NONE',  ( -1.000000000000000000, 0.000000000000000000, 0.000000000000000000 ) ) ;
#13287 = CARTESIAN_POINT ( 'NONE',  ( 3.034277558025862298, -9.029550313327863620, 2.543334857076493094 ) ) ;
#13288 = CARTESIAN_POINT ( 'NONE',  ( -14.49999999999998579, -19.49999999999999645, 4.000000000000000000 ) ) ;
#13289 = CARTESIAN_POINT ( 'NONE',  ( -12.62837453896009876, -19.32958578251692572, 4.742959489302074338 ) ) ;
#13290 = CARTESIAN_POINT ( 'NONE',  ( 5.402808582316794173, -22.77556120703056308, 1.770995438708340197 ) ) ;
#13291 = CARTESIAN_POINT ( 'NONE',  ( -4.000000000000000000, -12.50000000000000000, 1.000000000000000000 ) ) ;
#13292 = CARTESIAN_POINT ( 'NONE',  ( 13.12512971825177033, 5.006550771716304915, 5.133277049491872468 ) ) ;
#13293 = AXIS2_PLACEMENT_3D ( 'NONE', #12293, #6031, #12094 ) ;
#13294 = CARTESIAN_POINT ( 'NONE',  ( -0.5631383031621635116, -9.114917468222230923, 2.372643865078341019 ) ) ;
#13295 = CARTESIAN_POINT ( 'NONE',  ( 11.59030858231679595, -21.63647391050454871, 2.479004561291657804 ) ) ;
#13296 = CARTESIAN_POINT ( 'NONE',  ( 7.659691417683177406, -22.67418626127524917, 1.729004561291651809 ) ) ;
#13297 = CARTESIAN_POINT ( 'NONE',  ( -6.527808582316795949, -22.97900456129165647, 3.964901035250747885 ) ) ;
#13298 = EDGE_LOOP ( 'NONE', ( #16374, #4020, #19707, #12378 ) ) ;
#13299 = CARTESIAN_POINT ( 'NONE',  ( 12.92761177809936513, -5.718105205959081339, 6.548537912490751900 ) ) ;
#13300 = CARTESIAN_POINT ( 'NONE',  ( 13.09173631808601002, 4.070184063342107805, 5.250510817581989009 ) ) ;
#13301 = CARTESIAN_POINT ( 'NONE',  ( 11.49178095869207006, 9.000000000000001776, 1.000000000000000000 ) ) ;
#13302 = EDGE_LOOP ( 'NONE', ( #268, #12131, #13789, #18136 ) ) ;
#13303 = ORIENTED_EDGE ( 'NONE', *, *, #9648, .F. ) ;
#13304 = DIRECTION ( 'NONE',  ( -0.000000000000000000, -0.000000000000000000, -1.000000000000000000 ) ) ;
#13305 = VECTOR ( 'NONE', #10395, 1000.000000000000114 ) ;
#13306 = VECTOR ( 'NONE', #9183, 1000.000000000000000 ) ;
#13307 = EDGE_CURVE ( 'NONE', #12487, #1742, #8769, .T. ) ;
#13308 = DIRECTION ( 'NONE',  ( -0.000000000000000000, -0.000000000000000000, -1.000000000000000000 ) ) ;
#13309 = VECTOR ( 'NONE', #8834, 1000.000000000000000 ) ;
#13310 = VECTOR ( 'NONE', #10547, 1000.000000000000000 ) ;
#13311 = CARTESIAN_POINT ( 'NONE',  ( -3.997260319564023501, 4.999999999999999112, 1.000000000000000000 ) ) ;
#13312 = EDGE_CURVE ( 'NONE', #4104, #20490, #815, .T. ) ;
#13313 = CARTESIAN_POINT ( 'NONE',  ( -4.218479777801761976, -21.48426400496073541, 5.561508543513003389 ) ) ;
#13314 = CARTESIAN_POINT ( 'NONE',  ( 3.162271481458107658, -13.95306990448253437, 3.615178062515473911 ) ) ;
#13315 = FACE_OUTER_BOUND ( 'NONE', #2406, .T. ) ;
#13316 = EDGE_CURVE ( 'NONE', #4979, #14879, #3946, .T. ) ;
#13317 = CARTESIAN_POINT ( 'NONE',  ( -0.000000000000000000, 10.00000000000000000, 0.000000000000000000 ) ) ;
#13318 = CARTESIAN_POINT ( 'NONE',  ( 13.25392420457524878, -20.52600657937462358, 3.465375001445726966 ) ) ;
#13319 = CARTESIAN_POINT ( 'NONE',  ( 15.50000000000000178, -20.99999999999999645, 4.000000000000000000 ) ) ;
#13320 = CARTESIAN_POINT ( 'NONE',  ( -5.684058582316794173, -20.79840458871652942, 2.226721677130544030 ) ) ;
#13321 = AXIS2_PLACEMENT_3D ( 'NONE', #13473, #18404, #725 ) ;
#13322 = CARTESIAN_POINT ( 'NONE',  ( -1.337453470010121714, -8.364917468222230923, 2.372643865078341019 ) ) ;
#13323 = CIRCLE ( 'NONE', #15999, 10.00000000000000000 ) ;
#13324 = ORIENTED_EDGE ( 'NONE', *, *, #2999, .T. ) ;
#13325 = CARTESIAN_POINT ( 'NONE',  ( -13.38269957179998038, -19.11117162410040038, 4.745921838382382241 ) ) ;
#13326 = CARTESIAN_POINT ( 'NONE',  ( -7.559058582316794173, -20.72672167713054137, 4.701595411283463477 ) ) ;
#13327 = CARTESIAN_POINT ( 'NONE',  ( -8.409691417683177406, -21.32581373872474373, 5.270995438708348857 ) ) ;
#13328 = AXIS2_PLACEMENT_3D ( 'NONE', #4696, #15676, #4281 ) ;
#13329 = ORIENTED_EDGE ( 'NONE', *, *, #17901, .F. ) ;
#13330 = CARTESIAN_POINT ( 'NONE',  ( 13.38238173943565990, -19.87722215849730034, 5.285856107751903288 ) ) ;
#13331 = CARTESIAN_POINT ( 'NONE',  ( 0.000000000000000000, 4.999999999999999112, 0.000000000000000000 ) ) ;
#13332 = ORIENTED_EDGE ( 'NONE', *, *, #9414, .F. ) ;
#13333 = VECTOR ( 'NONE', #2562, 1000.000000000000000 ) ;
#13334 = ORIENTED_EDGE ( 'NONE', *, *, #12986, .F. ) ;
#13335 = DIRECTION ( 'NONE',  ( 1.000000000000000000, 0.000000000000000000, 0.000000000000000000 ) ) ;
#13336 = ORIENTED_EDGE ( 'NONE', *, *, #3802, .T. ) ;
#13337 = DIRECTION ( 'NONE',  ( 0.000000000000000000, -1.000000000000000000, 0.000000000000000000 ) ) ;
#13338 = EDGE_CURVE ( 'NONE', #9694, #17227, #7412, .T. ) ;
#13339 = VERTEX_POINT ( 'NONE', #5624 ) ;
#13340 = CARTESIAN_POINT ( 'NONE',  ( 7.003441417683177406, -22.05068747287765873, 5.250000000000000888 ) ) ;
#13341 = CARTESIAN_POINT ( 'NONE',  ( -21.42243175760212637, 9.000000000000001776, 1.000000000000000000 ) ) ;
#13342 =( REPRESENTATION_RELATIONSHIP ('NONE','NONE', #1880, #19662 ) REPRESENTATION_RELATIONSHIP_WITH_TRANSFORMATION ( #19965 )SHAPE_REPRESENTATION_RELATIONSHIP( ) );
#13343 = VECTOR ( 'NONE', #18338, 1000.000000000000000 ) ;
#13344 = CARTESIAN_POINT ( 'NONE',  ( -13.49999999999998401, -19.52007894294123957, 12.00000000000000000 ) ) ;
#13345 = CARTESIAN_POINT ( 'NONE',  ( 4.181771508648414404, -14.78356139460145968, 3.271079850667843125 ) ) ;
#13346 = CARTESIAN_POINT ( 'NONE',  ( -6.902808582316795061, -22.77556120703056308, 1.770995438708340197 ) ) ;
#13347 = CARTESIAN_POINT ( 'NONE',  ( 12.62499999999998224, -20.99999999999991829, 4.333333333333343695 ) ) ;
#13348 = DIRECTION ( 'NONE',  ( 1.000000000000000000, -0.000000000000000000, 0.000000000000000000 ) ) ;
#13349 = CARTESIAN_POINT ( 'NONE',  ( 12.15969141768317918, -22.36352608949543352, 2.479004561291652031 ) ) ;
#13350 = DIRECTION ( 'NONE',  ( 0.000000000000000000, -1.000000000000000000, 0.000000000000000000 ) ) ;
#13351 = EDGE_CURVE ( 'NONE', #2248, #15703, #10540, .T. ) ;
#13352 = CARTESIAN_POINT ( 'NONE',  ( -9.253441417683177406, -21.94931252712233061, 2.499999999999999112 ) ) ;
#13353 = CARTESIAN_POINT ( 'NONE',  ( -6.340308582316796837, -22.98484643305508612, 6.020995438708344416 ) ) ;
#13354 = VERTEX_POINT ( 'NONE', #20176 ) ;
#13355 = CARTESIAN_POINT ( 'NONE',  ( 13.10431844137356627, 3.955581289335645234, 6.006545679920360925 ) ) ;
#13356 = CARTESIAN_POINT ( 'NONE',  ( -12.62499999999998579, -20.24999999999999289, 3.146526952850934755 ) ) ;
#13357 = ORIENTED_EDGE ( 'NONE', *, *, #6332, .T. ) ;
#13358 = FACE_OUTER_BOUND ( 'NONE', #2782, .T. ) ;
#13359 = PLANE ( 'NONE',  #19366 ) ;
#13360 = VERTEX_POINT ( 'NONE', #4259 ) ;
#13361 = ORIENTED_EDGE ( 'NONE', *, *, #11213, .F. ) ;
#13362 = EDGE_CURVE ( 'NONE', #11847, #12998, #5837, .T. ) ;
#13363 = LINE ( 'NONE', #16504, #19164 ) ;
#13364 = EDGE_CURVE ( 'NONE', #11847, #18960, #9080, .T. ) ;
#13365 = ORIENTED_EDGE ( 'NONE', *, *, #9150, .F. ) ;
#13366 = PLANE ( 'NONE',  #304 ) ;
#13367 = CARTESIAN_POINT ( 'NONE',  ( 13.12119116326504908, 4.807653744879115010, 5.626470997801169105 ) ) ;
#13368 = CARTESIAN_POINT ( 'NONE',  ( -1.639793706121975614, -8.364901960018411131, 1.622639882261793343 ) ) ;
#13369 = CARTESIAN_POINT ( 'NONE',  ( 0.9854920305337621089, -9.114917468222230923, 2.372643865078341019 ) ) ;
#13370 = FACE_BOUND ( 'NONE', #15553, .T. ) ;
#13371 = DIRECTION ( 'NONE',  ( 0.000000000000000000, 1.000000000000000000, 0.000000000000000000 ) ) ;
#13372 = DIRECTION ( 'NONE',  ( -0.000000000000000000, -0.000000000000000000, -1.000000000000000000 ) ) ;
#13373 = VECTOR ( 'NONE', #12654, 1000.000000000000000 ) ;
#13374 = CARTESIAN_POINT ( 'NONE',  ( 11.59030858231679595, -21.01515356694490322, 0.9790045612916562501 ) ) ;
#13375 = CARTESIAN_POINT ( 'NONE',  ( -13.15498530132288479, 5.764257716805535559, 4.666666666666618113 ) ) ;
#13376 = EDGE_CURVE ( 'NONE', #13004, #1633, #9381, .T. ) ;
#13377 = CARTESIAN_POINT ( 'NONE',  ( -5.128441417683177406, -19.49999999999998934, 3.550687472877664952 ) ) ;
#13378 = VECTOR ( 'NONE', #17189, 1000.000000000000000 ) ;
#13379 = VECTOR ( 'NONE', #19943, 1000.000000000000000 ) ;
#13380 = DIRECTION ( 'NONE',  ( -0.000000000000000000, 0.000000000000000000, -1.000000000000000000 ) ) ;
#13381 = CARTESIAN_POINT ( 'NONE',  ( -14.99999999999998401, -25.49999999999999645, 1.000000000000000000 ) ) ;
#13382 = CARTESIAN_POINT ( 'NONE',  ( 6.715308582316796837, -23.02099543870833998, 3.136473910504556262 ) ) ;
#13383 = CARTESIAN_POINT ( 'NONE',  ( 11.99178095869207006, 0.000000000000000000, 1.000000000000000000 ) ) ;
#13384 = ORIENTED_EDGE ( 'NONE', *, *, #195, .F. ) ;
#13385 = VERTEX_POINT ( 'NONE', #10955 ) ;
#13386 = CARTESIAN_POINT ( 'NONE',  ( 13.37499999998404299, -20.99999999996810729, 2.793053905886972998 ) ) ;
#13387 = CARTESIAN_POINT ( 'NONE',  ( 0.000000000000000000, 10.00000000000000000, 1.000000000000000000 ) ) ;
#13388 = ORIENTED_EDGE ( 'NONE', *, *, #1360, .F. ) ;
#13389 = LINE ( 'NONE', #16623, #427 ) ;
#13390 = AXIS2_PLACEMENT_3D ( 'NONE', #4917, #9523, #19265 ) ;
#13391 = LINE ( 'NONE', #14859, #1358 ) ;
#13392 = CARTESIAN_POINT ( 'NONE',  ( 17.80017143803810242, 0.000000000000000000, 1.000000000000000000 ) ) ;
#13393 = AXIS2_PLACEMENT_3D ( 'NONE', #9978, #11550, #3598 ) ;
#13394 = CARTESIAN_POINT ( 'NONE',  ( 13.84863765609603625, 3.668701632846259830, 5.985835949623216301 ) ) ;
#13395 = AXIS2_PLACEMENT_3D ( 'NONE', #14555, #3373, #10912 ) ;
#13396 = DIRECTION ( 'NONE',  ( 0.000000000000000000, 0.000000000000000000, -1.000000000000000000 ) ) ;
#13397 = CARTESIAN_POINT ( 'NONE',  ( 3.537356407578672535, -11.36437789272258669, 3.142965222332344766 ) ) ;
#13398 = CARTESIAN_POINT ( 'NONE',  ( 17.12779268661489596, 10.00000000000000000, 0.000000000000000000 ) ) ;
#13399 = CARTESIAN_POINT ( 'NONE',  ( -13.01365964058540037, 0.1273118495903458325, 5.174178440007729307 ) ) ;
#13400 = LINE ( 'NONE', #14095, #15863 ) ;
#13401 = LINE ( 'NONE', #10168, #8731 ) ;
#13402 = CARTESIAN_POINT ( 'NONE',  ( 12.62524871736568954, -20.23743977303344010, 4.661898514667671023 ) ) ;
#13403 = EDGE_CURVE ( 'NONE', #1458, #458, #15552, .T. ) ;
#13404 = CARTESIAN_POINT ( 'NONE',  ( -1.548630333695928618, -9.864917468222230923, 2.372643865078341019 ) ) ;
#13405 = CARTESIAN_POINT ( 'NONE',  ( 9.152808582316795949, -21.53509896474924901, 4.479004561291659137 ) ) ;
#13406 = CIRCLE ( 'NONE', #4403, 10.00000000000000000 ) ;
#13407 = CARTESIAN_POINT ( 'NONE',  ( 6.909691417683177406, -21.32581373872474373, 5.270995438708348857 ) ) ;
#13408 = CARTESIAN_POINT ( 'NONE',  ( -8.965308582316794173, -20.22900456129164937, 4.174186261275266929 ) ) ;
#13409 = ORIENTED_EDGE ( 'NONE', *, *, #10847, .T. ) ;
#13410 = CARTESIAN_POINT ( 'NONE',  ( 13.13084019862132479, 4.544930030374419339, 6.677052771569639944 ) ) ;
#13411 = CARTESIAN_POINT ( 'NONE',  ( 12.64197948789552051, -18.64253586127677309, 4.770532606674187548 ) ) ;
#13412 = FACE_OUTER_BOUND ( 'NONE', #6850, .T. ) ;
#13413 = ORIENTED_EDGE ( 'NONE', *, *, #2254, .T. ) ;
#13414 = ORIENTED_EDGE ( 'NONE', *, *, #17526, .F. ) ;
#13415 = CARTESIAN_POINT ( 'NONE',  ( -17.94064177244175795, 10.00000000000000000, 1.000000000000000000 ) ) ;
#13416 = CARTESIAN_POINT ( 'NONE',  ( -7.499999999999999112, -18.49999999999999645, 6.500000000000000888 ) ) ;
#13417 = DIRECTION ( 'NONE',  ( 1.000000000000000000, 0.000000000000000000, 0.000000000000000000 ) ) ;
#13418 = CIRCLE ( 'NONE', #5764, 2.999999999999999112 ) ;
#13419 = DIRECTION ( 'NONE',  ( 0.000000000000000000, 1.000000000000000000, -0.000000000000000000 ) ) ;
#13420 = CARTESIAN_POINT ( 'NONE',  ( 2.559937518207947793, -9.746075135043517079, 2.534737762559237773 ) ) ;
#13421 = PLANE ( 'NONE',  #2368 ) ;
#13422 = LINE ( 'NONE', #5377, #19086 ) ;
#13423 = CARTESIAN_POINT ( 'NONE',  ( 12.75858672021238860, -20.53879859376904093, 3.532933081582447787 ) ) ;
#13424 = CARTESIAN_POINT ( 'NONE',  ( -15.61404127825609223, 9.000000000000001776, 1.000000000000000000 ) ) ;
#13425 = CARTESIAN_POINT ( 'NONE',  ( -8.309058582316792396, -23.27327832286945153, 2.298404588716537411 ) ) ;
#13426 = CARTESIAN_POINT ( 'NONE',  ( -3.486710468562268961, -9.848741751643258269, 2.003719583429115492 ) ) ;
#13427 = ORIENTED_EDGE ( 'NONE', *, *, #732, .T. ) ;
#13428 = CARTESIAN_POINT ( 'NONE',  ( -13.39169183355864590, -18.65706240528901105, 4.755687463382285429 ) ) ;
#13429 = AXIS2_PLACEMENT_3D ( 'NONE', #16325, #8485, #19893 ) ;
#13430 = CARTESIAN_POINT ( 'NONE',  ( -6.059058582316793284, -20.72672167713054137, 4.701595411283463477 ) ) ;
#13431 = EDGE_CURVE ( 'NONE', #3175, #95, #1232, .T. ) ;
#13432 = CARTESIAN_POINT ( 'NONE',  ( -11.03469141768317741, -20.97900456129164581, 3.136473910504570917 ) ) ;
#13433 = ORIENTED_EDGE ( 'NONE', *, *, #5064, .T. ) ;
#13434 = CARTESIAN_POINT ( 'NONE',  ( 13.39296152110871851, -19.34294318400601753, 5.489418334493660012 ) ) ;
#13435 = DIRECTION ( 'NONE',  ( 0.1351665943404306014, 0.9596796555888912339, -0.2464649070825229438 ) ) ;
#13436 = ORIENTED_EDGE ( 'NONE', *, *, #6466, .T. ) ;
#13437 = ORIENTED_EDGE ( 'NONE', *, *, #10759, .T. ) ;
#13438 = AXIS2_PLACEMENT_3D ( 'NONE', #6434, #12800, #19200 ) ;
#13439 = LINE ( 'NONE', #12081, #13379 ) ;
#13440 = VERTEX_POINT ( 'NONE', #15956 ) ;
#13441 = CARTESIAN_POINT ( 'NONE',  ( -13.37499999999998224, -20.24999999999991829, 4.333333333333343695 ) ) ;
#13442 = ADVANCED_FACE ( 'NONE', ( #4776 ), #6240, .T. ) ;
#13443 = ADVANCED_FACE ( 'NONE', ( #18809 ), #4670, .T. ) ;
#13444 = ORIENTED_EDGE ( 'NONE', *, *, #15750, .T. ) ;
#13445 = CARTESIAN_POINT ( 'NONE',  ( 4.472191417683177406, -23.72900456129164937, 2.724438792969417378 ) ) ;
#13446 = CARTESIAN_POINT ( 'NONE',  ( 2.311130159782011972, 0.000000000000000000, 1.000000000000000000 ) ) ;
#13447 = CARTESIAN_POINT ( 'NONE',  ( 11.00000000000000000, -18.49999999999999645, 4.000000000000000000 ) ) ;
#13448 = CARTESIAN_POINT ( 'NONE',  ( 1.619022621591186928, -8.364917468222230923, 2.372643865078341019 ) ) ;
#13449 = CARTESIAN_POINT ( 'NONE',  ( -5.871558582316794173, -20.24999999999999289, 3.449312527122348371 ) ) ;
#13450 = AXIS2_PLACEMENT_3D ( 'NONE', #16018, #3364, #20637 ) ;
#13451 = CARTESIAN_POINT ( 'NONE',  ( 12.62499999999998401, -20.99999999999999645, 3.666666666666654084 ) ) ;
#13452 = DIRECTION ( 'NONE',  ( 0.000000000000000000, 1.000000000000000000, 0.000000000000000000 ) ) ;
#13453 = CARTESIAN_POINT ( 'NONE',  ( 9.628441417683177406, -20.99999999999999645, 3.550687472877664952 ) ) ;
#13454 = CARTESIAN_POINT ( 'NONE',  ( -12.50209451496117197, 10.00000000000000000, 1.000000000000000000 ) ) ;
#13455 = CARTESIAN_POINT ( 'NONE',  ( -5.878441417683177406, -22.99999999999999645, 3.449312527122335048 ) ) ;
#13456 = ADVANCED_FACE ( 'NONE', ( #6044 ), #20588, .T. ) ;
#13457 = CARTESIAN_POINT ( 'NONE',  ( -8.402808582316797725, -23.08622137881038938, 1.020995438708339309 ) ) ;
#13458 = ORIENTED_EDGE ( 'NONE', *, *, #18197, .T. ) ;
#13459 = CARTESIAN_POINT ( 'NONE',  ( 12.62868952012632207, -19.31367923361656480, 4.748088538831167327 ) ) ;
#13460 = CARTESIAN_POINT ( 'NONE',  ( -12.95145221759166354, -3.764163011652346569, 5.840524842913703552 ) ) ;
#13461 = ORIENTED_EDGE ( 'NONE', *, *, #10626, .T. ) ;
#13462 = DIRECTION ( 'NONE',  ( -0.000000000000000000, 1.000000000000000000, -0.000000000000000000 ) ) ;
#13463 = DIRECTION ( 'NONE',  ( -1.000000000000000000, 0.000000000000000000, 0.000000000000000000 ) ) ;
#13464 = ORIENTED_EDGE ( 'NONE', *, *, #4912, .T. ) ;
#13465 = ORIENTED_EDGE ( 'NONE', *, *, #13218, .F. ) ;
#13466 = VECTOR ( 'NONE', #6019, 1000.000000000000000 ) ;
#13467 = CARTESIAN_POINT ( 'NONE',  ( -13.50000000000000178, 0.000000000000000000, 1.000000000000000000 ) ) ;
#13468 = ORIENTED_EDGE ( 'NONE', *, *, #20628, .T. ) ;
#13469 = EDGE_CURVE ( 'NONE', #5573, #14252, #20380, .T. ) ;
#13470 = CARTESIAN_POINT ( 'NONE',  ( -11.75209451496117197, 10.00000000000000000, 1.000000000000000000 ) ) ;
#13471 = CARTESIAN_POINT ( 'NONE',  ( 13.12529397354238192, 5.014845663890297622, 3.999999999999981792 ) ) ;
#13472 = CARTESIAN_POINT ( 'NONE',  ( -1.619022621591186928, -8.364917468222230923, 1.622643865078341907 ) ) ;
#13473 = CARTESIAN_POINT ( 'NONE',  ( 6.813547257480585095, 0.000000000000000000, 1.000000000000000000 ) ) ;
#13474 = LINE ( 'NONE', #8567, #3143 ) ;
#13475 = CARTESIAN_POINT ( 'NONE',  ( 13.10557919622060652, 4.019249409169220577, 6.007898877577752650 ) ) ;
#13476 = CARTESIAN_POINT ( 'NONE',  ( -12.50209451496117197, 0.000000000000000000, 1.000000000000000000 ) ) ;
#13477 = CARTESIAN_POINT ( 'NONE',  ( 9.909691417683175629, -21.01515356694492098, 6.020995438708349745 ) ) ;
#13478 = CARTESIAN_POINT ( 'NONE',  ( -12.65051119073526564, -18.96168486786632457, 5.513701926248478102 ) ) ;
#13479 = CARTESIAN_POINT ( 'NONE',  ( -6.440941417683175629, -20.19639159124061933, 1.768074502826635586 ) ) ;
#13480 = EDGE_CURVE ( 'NONE', #12338, #995, #17323, .T. ) ;
#13481 = VERTEX_POINT ( 'NONE', #9277 ) ;
#13482 = EDGE_CURVE ( 'NONE', #6507, #995, #7607, .T. ) ;
#13483 = DIRECTION ( 'NONE',  ( 0.000000000000000000, 0.000000000000000000, 1.000000000000000000 ) ) ;
#13484 = PLANE ( 'NONE',  #6748 ) ;
#13485 = CARTESIAN_POINT ( 'NONE',  ( -13.41355111217617413, -19.05316883510194614, 6.247234435864091218 ) ) ;
#13486 = CARTESIAN_POINT ( 'NONE',  ( 5.215308582316795949, -23.02099543870833998, 3.136473910504556262 ) ) ;
#13487 = LINE ( 'NONE', #2294, #18344 ) ;
#13488 = ORIENTED_EDGE ( 'NONE', *, *, #18048, .F. ) ;
#13489 = VERTEX_POINT ( 'NONE', #13975 ) ;
#13490 = CARTESIAN_POINT ( 'NONE',  ( 13.83065313257865370, 2.760483195222930952, 5.966304699623404595 ) ) ;
#13491 = VECTOR ( 'NONE', #10399, 1000.000000000000000 ) ;
#13492 = CARTESIAN_POINT ( 'NONE',  ( -3.499999999999998668, -19.50000000000000000, 4.000000000000000000 ) ) ;
#13493 = SURFACE_STYLE_FILL_AREA ( #7130 ) ;
#13494 = ORIENTED_EDGE ( 'NONE', *, *, #14213, .F. ) ;
#13495 = DIRECTION ( 'NONE',  ( 1.000000000000000000, 0.000000000000000000, 0.000000000000000000 ) ) ;
#13496 = CARTESIAN_POINT ( 'NONE',  ( 10.00000000000000355, -34.99999999999999289, 1.000000000000000000 ) ) ;
#13497 = EDGE_CURVE ( 'NONE', #17944, #12390, #7298, .T. ) ;
#13498 = LINE ( 'NONE', #2510, #4622 ) ;
#13499 = CARTESIAN_POINT ( 'NONE',  ( 13.39902456816392906, -19.03675930772010361, 5.497554699623231400 ) ) ;
#13500 = DIRECTION ( 'NONE',  ( -1.000000000000000000, 0.000000000000000000, 0.000000000000000000 ) ) ;
#13501 = CARTESIAN_POINT ( 'NONE',  ( 3.722205087890566144, -11.52065056559861134, 2.433099166587254558 ) ) ;
#13502 = DIRECTION ( 'NONE',  ( -0.000000000000000000, -0.000000000000000000, -1.000000000000000000 ) ) ;
#13503 = CARTESIAN_POINT ( 'NONE',  ( -13.12529397354238192, 5.014845663890295846, 4.166666666666765551 ) ) ;
#13504 = CARTESIAN_POINT ( 'NONE',  ( 25.37918902992234393, 11.64110105645932691, 0.000000000000000000 ) ) ;
#13505 = DIRECTION ( 'NONE',  ( 1.000000000000000000, 0.000000000000000000, 0.000000000000000000 ) ) ;
#13506 = CARTESIAN_POINT ( 'NONE',  ( -13.87470602645761986, 4.985154336109792972, 3.666666666666500873 ) ) ;
#13507 = EDGE_CURVE ( 'NONE', #16884, #19883, #20688, .T. ) ;
#13508 = CARTESIAN_POINT ( 'NONE',  ( 13.50000000000000178, 5.000000000000047962, 4.000000000000000000 ) ) ;
#13509 = CARTESIAN_POINT ( 'NONE',  ( 9.340308582316795949, -22.36352608949544418, 4.520995438708343528 ) ) ;
#13510 = CARTESIAN_POINT ( 'NONE',  ( 6.440941417683176518, -20.72672167713052715, 2.298404588716546293 ) ) ;
#13511 = CARTESIAN_POINT ( 'NONE',  ( -10.93405858231679417, -23.20159541128345992, 4.773278322869455970 ) ) ;
#13512 = ORIENTED_EDGE ( 'NONE', *, *, #2983, .F. ) ;
#13513 = CARTESIAN_POINT ( 'NONE',  ( 13.10985494974158705, 3.485174961951963191, 6.746454579156001330 ) ) ;
#13514 = CARTESIAN_POINT ( 'NONE',  ( 12.62746768552656285, -19.37538188090202596, 4.723115281690125400 ) ) ;
#13515 = DIRECTION ( 'NONE',  ( 0.000000000000000000, 1.000000000000000000, -1.304178812473495102E-15 ) ) ;
#13516 = VERTEX_POINT ( 'NONE', #19123 ) ;
#13517 = ORIENTED_EDGE ( 'NONE', *, *, #17734, .T. ) ;
#13518 = DIRECTION ( 'NONE',  ( 1.000000000000000000, 0.000000000000000000, 0.000000000000000000 ) ) ;
#13519 = EDGE_CURVE ( 'NONE', #14797, #9402, #2901, .T. ) ;
#13520 = CYLINDRICAL_SURFACE ( 'NONE', #13251, 10.00000000000000000 ) ;
#13521 = CARTESIAN_POINT ( 'NONE',  ( 12.25209451496117197, 0.000000000000000000, 0.000000000000000000 ) ) ;
#13522 = LINE ( 'NONE', #19924, #13001 ) ;
#13523 = CARTESIAN_POINT ( 'NONE',  ( 2.534747216115884161, -9.671180236796224960, 2.515503256513427210 ) ) ;
#13524 = DIRECTION ( 'NONE',  ( 0.000000000000000000, 0.000000000000000000, 1.000000000000000000 ) ) ;
#13525 = DIRECTION ( 'NONE',  ( -0.000000000000000000, -0.000000000000000000, -1.000000000000000000 ) ) ;
#13526 = CARTESIAN_POINT ( 'NONE',  ( 12.93483012243689068, -20.62499177937328199, 3.508889823513372086 ) ) ;
#13527 = CARTESIAN_POINT ( 'NONE',  ( -2.596731678114175157, -9.937710376390764822, 2.583953520835782225 ) ) ;
#13528 = CARTESIAN_POINT ( 'NONE',  ( -5.777808582316794173, -20.27099543870833642, 2.724438792969431589 ) ) ;
#13529 = CARTESIAN_POINT ( 'NONE',  ( -3.451003380014874722, -9.682417022083358304, 1.961004070207825523 ) ) ;
#13530 = ORIENTED_EDGE ( 'NONE', *, *, #1596, .T. ) ;
#13531 = CARTESIAN_POINT ( 'NONE',  ( -13.37500000000002132, -19.50000000000273559, 4.083333333315724012 ) ) ;
#13532 = CARTESIAN_POINT ( 'NONE',  ( -5.684058582316794173, -20.79840458871652942, 2.226721677130544030 ) ) ;
#13533 = CARTESIAN_POINT ( 'NONE',  ( 10.74655858231679595, -21.94931252712234127, 6.000000000000001776 ) ) ;
#13534 = CARTESIAN_POINT ( 'NONE',  ( -12.15969141768317918, -22.36352608949543352, 2.479004561291652031 ) ) ;
#13535 = VERTEX_POINT ( 'NONE', #7915 ) ;
#13536 = CARTESIAN_POINT ( 'NONE',  ( 13.40621837757088564, -18.67347193267085714, 5.505367199623145247 ) ) ;
#13537 = CARTESIAN_POINT ( 'NONE',  ( -15.49999999999998046, -26.49999999999999645, 1.000000000000000000 ) ) ;
#13538 = VERTEX_POINT ( 'NONE', #1337 ) ;
#13539 = VECTOR ( 'NONE', #17276, 1000.000000000000000 ) ;
#13540 = ORIENTED_EDGE ( 'NONE', *, *, #1596, .F. ) ;
#13541 = CARTESIAN_POINT ( 'NONE',  ( 23.31633994409548549, 16.00000000000000000, 1.000000000000000000 ) ) ;
#13542 = VERTEX_POINT ( 'NONE', #3006 ) ;
#13543 = DIRECTION ( 'NONE',  ( 0.000000000000000000, 0.000000000000000000, 1.000000000000000000 ) ) ;
#13544 = EDGE_LOOP ( 'NONE', ( #3894, #18805, #881, #17203 ) ) ;
#13545 = PLANE ( 'NONE',  #7535 ) ;
#13546 = CARTESIAN_POINT ( 'NONE',  ( -11.24178095869206828, 4.999999999999999112, 1.000000000000000000 ) ) ;
#13547 = ADVANCED_FACE ( 'NONE', ( #9177 ), #20491, .F. ) ;
#13548 = CYLINDRICAL_SURFACE ( 'NONE', #4969, 59.99999999999998579 ) ;
#13549 = CARTESIAN_POINT ( 'NONE',  ( 1.126276606324276619, -9.114917468222230923, 2.372643865078341019 ) ) ;
#13550 = CARTESIAN_POINT ( 'NONE',  ( -6.809058582316794173, -23.27327832286945153, 2.298404588716537411 ) ) ;
#13551 = CARTESIAN_POINT ( 'NONE',  ( 12.62499963760179256, -21.00001830110826972, 4.442557003548452066 ) ) ;
#13552 = FACE_OUTER_BOUND ( 'NONE', #17629, .T. ) ;
#13553 = CARTESIAN_POINT ( 'NONE',  ( 4.753441417683176518, -21.94931252712233061, 1.749999999999998446 ) ) ;
#13554 = CARTESIAN_POINT ( 'NONE',  ( -14.49999999999998579, -19.49999999999999645, 4.000000000000000000 ) ) ;
#13555 = CARTESIAN_POINT ( 'NONE',  ( -4.940941417683177406, -21.25705176302044208, 2.828734674606458555 ) ) ;
#13556 = CARTESIAN_POINT ( 'NONE',  ( -4.840308582316795061, -22.98484643305508612, 6.020995438708344416 ) ) ;
#13557 = ORIENTED_EDGE ( 'NONE', *, *, #2620, .T. ) ;
#13558 = CARTESIAN_POINT ( 'NONE',  ( 12.62837453896009876, -19.32958578251692572, 4.742959489302074338 ) ) ;
#13559 = CARTESIAN_POINT ( 'NONE',  ( -13.08573665985359824, 3.017201322601628100, 5.986358176248492313 ) ) ;
#13560 = ORIENTED_EDGE ( 'NONE', *, *, #20280, .T. ) ;
#13561 = DIRECTION ( 'NONE',  ( 5.204170427930446527E-15, -1.000000000000000000, 0.000000000000000000 ) ) ;
#13562 = DIRECTION ( 'NONE',  ( 0.000000000000000000, -1.000000000000000000, 0.000000000000000000 ) ) ;
#13563 = VERTEX_POINT ( 'NONE', #1440 ) ;
#13564 = VERTEX_POINT ( 'NONE', #7818 ) ;
#13565 = ORIENTED_EDGE ( 'NONE', *, *, #8488, .F. ) ;
#13566 = CARTESIAN_POINT ( 'NONE',  ( 13.50000000000001243, -18.49999999999999645, 1.000000000000000000 ) ) ;
#13567 = LINE ( 'NONE', #12006, #7967 ) ;
#13568 = EDGE_CURVE ( 'NONE', #18720, #11223, #19016, .T. ) ;
#13569 = CARTESIAN_POINT ( 'NONE',  ( -2.226467333542268445, -8.440126719678968215, 1.641959103308203716 ) ) ;
#13570 = CARTESIAN_POINT ( 'NONE',  ( -13.49999999999998401, -24.49999999999999289, 4.000000000000000000 ) ) ;
#13571 = LINE ( 'NONE', #2184, #11805 ) ;
#13572 = DIRECTION ( 'NONE',  ( 0.4999999999999950040, -0.8660254037844415942, 0.000000000000000000 ) ) ;
#13573 = EDGE_CURVE ( 'NONE', #3633, #13083, #15856, .T. ) ;
#13574 = EDGE_CURVE ( 'NONE', #4233, #7302, #12720, .T. ) ;
#13575 = CARTESIAN_POINT ( 'NONE',  ( 12.62844141768317741, -19.49999999999998934, 3.550687472877664952 ) ) ;
#13576 = CARTESIAN_POINT ( 'NONE',  ( -12.64323021897839006, -19.32937394158751943, 5.504219675487169283 ) ) ;
#13577 = CARTESIAN_POINT ( 'NONE',  ( -9.065941417683177406, -23.73192549717336064, 1.696391591240623331 ) ) ;
#13578 = EDGE_LOOP ( 'NONE', ( #13800, #18522, #8014, #7785 ) ) ;
#13579 = DIRECTION ( 'NONE',  ( 0.000000000000000000, 0.000000000000000000, 1.000000000000000000 ) ) ;
#13580 = CARTESIAN_POINT ( 'NONE',  ( -5.000000000000000000, -7.500000000000000000, 1.000000000000000000 ) ) ;
#13581 = CARTESIAN_POINT ( 'NONE',  ( -13.87005939078915873, 4.000499234880882327, 6.742989431566016378 ) ) ;
#13582 = EDGE_CURVE ( 'NONE', #1441, #14649, #2152, .T. ) ;
#13583 = CARTESIAN_POINT ( 'NONE',  ( 12.43405858231679417, -23.20159541128345992, 4.773278322869455970 ) ) ;
#13584 = CARTESIAN_POINT ( 'NONE',  ( -17.55017143803810242, 0.000000000000000000, 1.000000000000000000 ) ) ;
#13585 = ORIENTED_EDGE ( 'NONE', *, *, #1166, .F. ) ;
#13586 = ORIENTED_EDGE ( 'NONE', *, *, #11698, .T. ) ;
#13587 = CARTESIAN_POINT ( 'NONE',  ( 13.39170256340046095, -19.40652054827866380, 5.481861153867630065 ) ) ;
#13588 = CARTESIAN_POINT ( 'NONE',  ( 9.000000000000000000, -9.999999999999991118, 2.500000000000000000 ) ) ;
#13589 = EDGE_LOOP ( 'NONE', ( #19032, #5936, #15219, #14081, #15837 ) ) ;
#13590 = LINE ( 'NONE', #4188, #9461 ) ;
#13591 = CIRCLE ( 'NONE', #2581, 10.00000000000000000 ) ;
#13592 = CARTESIAN_POINT ( 'NONE',  ( 8.126396343307449754, 10.00000000000000000, 0.000000000000000000 ) ) ;
#13593 = FACE_OUTER_BOUND ( 'NONE', #2357, .T. ) ;
#13594 = DIRECTION ( 'NONE',  ( -1.000000000000000000, 0.000000000000000000, 0.000000000000000000 ) ) ;
#13595 = EDGE_CURVE ( 'NONE', #11608, #20520, #13031, .T. ) ;
#13596 = FACE_OUTER_BOUND ( 'NONE', #16977, .T. ) ;
#13597 = CARTESIAN_POINT ( 'NONE',  ( 3.607313482701580476, -10.70492285834919244, 2.223603995567122293 ) ) ;
#13598 = CARTESIAN_POINT ( 'NONE',  ( -13.67791111847408025, 0.000000000000000000, 0.000000000000000000 ) ) ;
#13599 = CARTESIAN_POINT ( 'NONE',  ( -13.12529397354238192, 5.014845663890295846, 3.000000000000000000 ) ) ;
#13600 = DIRECTION ( 'NONE',  ( 0.000000000000000000, 1.000000000000000000, 0.000000000000000000 ) ) ;
#13601 = CARTESIAN_POINT ( 'NONE',  ( 11.49655858231679417, -22.05068747287764452, 1.749999999999998446 ) ) ;
#13602 = CARTESIAN_POINT ( 'NONE',  ( -13.37499964066394043, -21.00001814646822496, 4.442866346476199269 ) ) ;
#13603 = FACE_OUTER_BOUND ( 'NONE', #9794, .T. ) ;
#13604 = CARTESIAN_POINT ( 'NONE',  ( 4.934058582316795061, -22.67126532539354855, 4.242948236979545484 ) ) ;
#13605 = EDGE_CURVE ( 'NONE', #13273, #607, #3724, .T. ) ;
#13606 = CARTESIAN_POINT ( 'NONE',  ( 4.847191417683178294, -21.22443879296941915, 1.770995438708345748 ) ) ;
#13607 = CARTESIAN_POINT ( 'NONE',  ( -13.18405858231679417, -20.79840458871652942, 2.226721677130544030 ) ) ;
#13608 = EDGE_LOOP ( 'NONE', ( #13720, #6558, #13201, #16672 ) ) ;
#13609 = CARTESIAN_POINT ( 'NONE',  ( 13.09546733092777160, 2.758600211853326822, 6.730829579156167419 ) ) ;
#13610 = CARTESIAN_POINT ( 'NONE',  ( 12.62599452815238443, -19.44977632830967806, 4.656396506304353977 ) ) ;
#13611 = DIRECTION ( 'NONE',  ( -3.469446951953611033E-15, 1.000000000000000000, 0.000000000000000000 ) ) ;
#13612 = ORIENTED_EDGE ( 'NONE', *, *, #8976, .T. ) ;
#13613 = ORIENTED_EDGE ( 'NONE', *, *, #5016, .T. ) ;
#13614 = LINE ( 'NONE', #17176, #11444 ) ;
#13615 = DIRECTION ( 'NONE',  ( -1.000000000000000000, 0.000000000000000000, 0.000000000000000000 ) ) ;
#13616 = EDGE_CURVE ( 'NONE', #3941, #13949, #12921, .T. ) ;
#13617 = EDGE_CURVE ( 'NONE', #351, #13057, #17945, .T. ) ;
#13618 = DIRECTION ( 'NONE',  ( 0.000000000000000000, -1.000000000000000000, 0.000000000000000000 ) ) ;
#13619 = CARTESIAN_POINT ( 'NONE',  ( 14.49999999999998579, -25.49999999999999645, 4.000000000000000000 ) ) ;
#13620 = CARTESIAN_POINT ( 'NONE',  ( 0.2815691515810352930, -9.114917468222230923, 2.372643865078523984 ) ) ;
#13621 = LINE ( 'NONE', #15406, #17846 ) ;
#13622 = PLANE ( 'NONE',  #711 ) ;
#13623 = CARTESIAN_POINT ( 'NONE',  ( -4.999999999999998224, 0.000000000000000000, 9.999999999999998224 ) ) ;
#13624 = CARTESIAN_POINT ( 'NONE',  ( -10.55905858231679595, -20.19639159124062999, 5.231925497173373074 ) ) ;
#13625 = CARTESIAN_POINT ( 'NONE',  ( -2.532303758294933704, -8.551221675625164664, 1.670490507339845054 ) ) ;
#13626 = EDGE_LOOP ( 'NONE', ( #5343, #18572, #19787, #15620, #4074, #3815, #12970, #14077, #914, #4774, #9823, #18879, #1996, #7125 ) ) ;
#13627 = CARTESIAN_POINT ( 'NONE',  ( -13.39888564296547635, -18.29377503024027263, 4.763499963382565205 ) ) ;
#13628 = CARTESIAN_POINT ( 'NONE',  ( -9.246558582316794173, -21.94931252712234482, 5.250000000000000888 ) ) ;
#13629 = EDGE_CURVE ( 'NONE', #5929, #6320, #8534, .T. ) ;
#13630 = CARTESIAN_POINT ( 'NONE',  ( 9.534691417683177406, -19.47900456129164581, 2.515153566944927199 ) ) ;
#13631 = CARTESIAN_POINT ( 'NONE',  ( -8.972191417683177406, -22.97900456129165292, 3.035098964749240125 ) ) ;
#13632 = ORIENTED_EDGE ( 'NONE', *, *, #18198, .F. ) ;
#13633 = CARTESIAN_POINT ( 'NONE',  ( 13.84863765609603625, 3.668701632846259830, 5.985835949623216301 ) ) ;
#13634 = LINE ( 'NONE', #13745, #10388 ) ;
#13635 = VERTEX_POINT ( 'NONE', #3416 ) ;
#13636 = AXIS2_PLACEMENT_3D ( 'NONE', #7725, #8030, #16084 ) ;
#13637 = ORIENTED_EDGE ( 'NONE', *, *, #12365, .F. ) ;
#13638 = CARTESIAN_POINT ( 'NONE',  ( 20.50349085826861995, 0.000000000000000000, 1.000000000000000000 ) ) ;
#13639 = ORIENTED_EDGE ( 'NONE', *, *, #417, .F. ) ;
#13640 = CARTESIAN_POINT ( 'NONE',  ( -13.37499979530394967, -20.25001033714808329, 4.458488164327452097 ) ) ;
#13641 = ORIENTED_EDGE ( 'NONE', *, *, #7472, .T. ) ;
#13642 = CARTESIAN_POINT ( 'NONE',  ( -14.49999999999998579, -19.52007894294123957, 12.00000000000000000 ) ) ;
#13643 = DIRECTION ( 'NONE',  ( 0.000000000000000000, -1.000000000000000000, 0.000000000000000000 ) ) ;
#13644 = DIRECTION ( 'NONE',  ( -0.000000000000000000, -0.000000000000000000, -1.000000000000000000 ) ) ;
#13645 = CLOSED_SHELL ( 'NONE', ( #5426, #17692, #16399, #8273, #13442, #16767, #8210, #8095, #12765, #20591, #19263, #19734, #7368, #11188, #3900, #5528, #10541, #10834, #10959, #987, #16192, #16256, #9701, #13855, #14120, #2515, #14653, #14238, #10340, #34, #7984, #19280, #16021, #637, #13172, #17544, #8509, #7211, #4861, #10944, #12906, #19529, #8206, #926, #17194, #17455, #9497, #3933, #14158, #13837, #5318, #2456, #18507, #8612, #6928 ) ) ;
#13646 = CARTESIAN_POINT ( 'NONE',  ( 1.824488249492779879, -9.124319963227819130, 2.375058613629473570 ) ) ;
#13647 = LINE ( 'NONE', #15326, #9860 ) ;
#13648 = CARTESIAN_POINT ( 'NONE',  ( 12.64183575740756993, -20.14979425091403087, 6.022201559249563907 ) ) ;
#13649 = AXIS2_PLACEMENT_3D ( 'NONE', #13253, #13463, #2077 ) ;
#13650 = LINE ( 'NONE', #8546, #1614 ) ;
#13651 = CARTESIAN_POINT ( 'NONE',  ( 0.000000000000000000, 9.000000000000000000, 0.000000000000000000 ) ) ;
#13652 = CARTESIAN_POINT ( 'NONE',  ( 5.690941417683176518, -23.27327832286946219, 4.701595411283453707 ) ) ;
#13653 = DIRECTION ( 'NONE',  ( 0.000000000000000000, -1.000000000000000000, 0.000000000000000000 ) ) ;
#13654 = CARTESIAN_POINT ( 'NONE',  ( -9.440941417683177406, -21.25705176302044208, 2.828734674606458555 ) ) ;
#13655 = ADVANCED_FACE ( 'NONE', ( #17634 ), #1944, .F. ) ;
#13656 = CARTESIAN_POINT ( 'NONE',  ( -11.12844141768317741, -19.49999999999998934, 3.550687472877664952 ) ) ;
#13657 = ORIENTED_EDGE ( 'NONE', *, *, #10520, .T. ) ;
#13658 = CARTESIAN_POINT ( 'NONE',  ( 12.63598464672302590, -18.94527534048458151, 4.764022190007618285 ) ) ;
#13659 = FACE_OUTER_BOUND ( 'NONE', #4828, .T. ) ;
#13660 = ORIENTED_EDGE ( 'NONE', *, *, #16581, .T. ) ;
#13661 = CARTESIAN_POINT ( 'NONE',  ( 17.12779268661489596, 0.000000000000000000, 0.000000000000000000 ) ) ;
#13662 = CARTESIAN_POINT ( 'NONE',  ( -14.49999999999998579, -18.49999999999999645, 4.000000000000000000 ) ) ;
#13663 = ORIENTED_EDGE ( 'NONE', *, *, #4983, .F. ) ;
#13664 = AXIS2_PLACEMENT_3D ( 'NONE', #363, #8515, #6842 ) ;
#13665 = ORIENTED_EDGE ( 'NONE', *, *, #20684, .T. ) ;
#13666 = AXIS2_PLACEMENT_3D ( 'NONE', #15341, #12585, #8105 ) ;
#13667 = AXIS2_PLACEMENT_3D ( 'NONE', #7288, #4465, #10850 ) ;
#13668 = ORIENTED_EDGE ( 'NONE', *, *, #11946, .F. ) ;
#13669 = CARTESIAN_POINT ( 'NONE',  ( -10.38119784648305632, -14.00000000000000000, 2.000000000000000000 ) ) ;
#13670 = DIRECTION ( 'NONE',  ( 1.000000000000000000, 0.000000000000000000, 0.000000000000000000 ) ) ;
#13671 = CARTESIAN_POINT ( 'NONE',  ( -2.309828811027716977, -9.292785183284841821, 1.668323847571005603 ) ) ;
#13672 = LINE ( 'NONE', #15458, #17710 ) ;
#13673 = LINE ( 'NONE', #13784, #6639 ) ;
#13674 = LINE ( 'NONE', #2708, #10026 ) ;
#13675 = VECTOR ( 'NONE', #19283, 1000.000000000000000 ) ;
#13676 = CARTESIAN_POINT ( 'NONE',  ( 10.19094141768317741, -23.80360840875937001, 5.231925497173365081 ) ) ;
#13677 = CARTESIAN_POINT ( 'NONE',  ( -12.64571531779736979, -19.20387645123237164, 5.508493592915143289 ) ) ;
#13678 = CARTESIAN_POINT ( 'NONE',  ( -5.409691417683178294, -21.01515356694492098, 6.020995438708349745 ) ) ;
#13679 = VERTEX_POINT ( 'NONE', #14905 ) ;
#13680 = CARTESIAN_POINT ( 'NONE',  ( 11.49655858231679417, -22.05068747287764452, 1.749999999999998446 ) ) ;
#13681 = DIRECTION ( 'NONE',  ( 1.000000000000000000, 0.000000000000000000, 0.000000000000000000 ) ) ;
#13682 = CARTESIAN_POINT ( 'NONE',  ( -13.85716935893578317, 3.349552626256921517, 6.729005269197402939 ) ) ;
#13683 = VECTOR ( 'NONE', #14629, 1000.000000000000000 ) ;
#13684 = ADVANCED_FACE ( 'NONE', ( #6962 ), #19534, .T. ) ;
#13685 = CARTESIAN_POINT ( 'NONE',  ( 10.93405858231679417, -23.20159541128345992, 4.773278322869455970 ) ) ;
#13686 = PLANE ( 'NONE',  #19688 ) ;
#13687 = ORIENTED_EDGE ( 'NONE', *, *, #7123, .F. ) ;
#13688 = VERTEX_POINT ( 'NONE', #14702 ) ;
#13689 = CARTESIAN_POINT ( 'NONE',  ( 13.87470623115321899, 4.985164673244912414, 4.958488177337359026 ) ) ;
#13690 = CARTESIAN_POINT ( 'NONE',  ( -8.376396343307449754, 10.00000000000000000, 1.000000000000000000 ) ) ;
#13691 = ORIENTED_EDGE ( 'NONE', *, *, #3557, .F. ) ;
#13692 = LINE ( 'NONE', #12136, #7795 ) ;
#13693 = EDGE_CURVE ( 'NONE', #18235, #9195, #18055, .T. ) ;
#13694 = AXIS2_PLACEMENT_3D ( 'NONE', #5746, #825, #2487 ) ;
#13695 = EDGE_CURVE ( 'NONE', #1231, #1866, #4980, .T. ) ;
#13696 = DIRECTION ( 'NONE',  ( 0.000000000000000000, -1.000000000000000000, 0.000000000000000000 ) ) ;
#13697 = CARTESIAN_POINT ( 'NONE',  ( -11.02780858231679595, -23.72900456129165647, 4.275561207030568411 ) ) ;
#13698 = DIRECTION ( 'NONE',  ( -1.000000000000000000, 0.000000000000000000, 0.000000000000000000 ) ) ;
#13699 = AXIS2_PLACEMENT_3D ( 'NONE', #5877, #12247, #2841 ) ;
#13700 = CARTESIAN_POINT ( 'NONE',  ( 0.000000000000000000, 9.000000000000001776, 1.000000000000000000 ) ) ;
#13701 = CARTESIAN_POINT ( 'NONE',  ( 0.5631383031621635116, -8.364917468222230923, 1.622643865078341907 ) ) ;
#13702 = VECTOR ( 'NONE', #16329, 1000.000000000000000 ) ;
#13703 = VECTOR ( 'NONE', #10307, 1000.000000000000000 ) ;
#13704 = DIRECTION ( 'NONE',  ( 1.156482317317871133E-15, -1.000000000000000000, 0.000000000000000000 ) ) ;
#13705 = CARTESIAN_POINT ( 'NONE',  ( -13.09560264576187905, 4.265433610975056133, 4.833333333333343695 ) ) ;
#13706 = CARTESIAN_POINT ( 'NONE',  ( 10.37155858231679417, -20.24999999999999289, 3.449312527122348371 ) ) ;
#13707 = CARTESIAN_POINT ( 'NONE',  ( -13.85716935893578317, 3.349552626256921517, 6.729005269197402939 ) ) ;
#13708 = DIRECTION ( 'NONE',  ( 0.000000000000000000, 0.000000000000000000, 1.000000000000000000 ) ) ;
#13709 = CARTESIAN_POINT ( 'NONE',  ( 13.18405858231679417, -20.79840458871652942, 2.226721677130544030 ) ) ;
#13710 = EDGE_CURVE ( 'NONE', #20155, #3140, #1748, .T. ) ;
#13711 = CARTESIAN_POINT ( 'NONE',  ( 4.753441417683176518, -21.94931252712233061, 1.749999999999998446 ) ) ;
#13712 = CARTESIAN_POINT ( 'NONE',  ( -11.40280858231679417, -22.77556120703056308, 1.770995438708339975 ) ) ;
#13713 = ORIENTED_EDGE ( 'NONE', *, *, #1313, .F. ) ;
#13714 = CARTESIAN_POINT ( 'NONE',  ( 12.63598464672302590, -18.94527534048458151, 4.764022190007618285 ) ) ;
#13715 = CARTESIAN_POINT ( 'NONE',  ( 1.937849085826861328, 0.000000000000000000, 1.000000000000000000 ) ) ;
#13716 = VECTOR ( 'NONE', #16073, 1000.000000000000000 ) ;
#13717 = ORIENTED_EDGE ( 'NONE', *, *, #8398, .F. ) ;
#13718 = VECTOR ( 'NONE', #11753, 1000.000000000000000 ) ;
#13719 = AXIS2_PLACEMENT_3D ( 'NONE', #340, #18122, #6724 ) ;
#13720 = ORIENTED_EDGE ( 'NONE', *, *, #1977, .T. ) ;
#13721 = DIRECTION ( 'NONE',  ( 1.000000000000000000, 0.000000000000000000, 0.000000000000000000 ) ) ;
#13722 = VECTOR ( 'NONE', #13335, 1000.000000000000000 ) ;
#13723 = CARTESIAN_POINT ( 'NONE',  ( -12.62500000000001954, -20.24999999999506173, 3.850307403176420618 ) ) ;
#13724 = CARTESIAN_POINT ( 'NONE',  ( -2.817596665886821672, -11.50588678273290988, 2.986692549455723267 ) ) ;
#13725 = CARTESIAN_POINT ( 'NONE',  ( -13.85593616229004610, 4.037276195647738319, 5.992122970672676630 ) ) ;
#13726 = ADVANCED_FACE ( 'NONE', ( #8131 ), #11468, .T. ) ;
#13727 = LINE ( 'NONE', #13619, #8717 ) ;
#13728 = CARTESIAN_POINT ( 'NONE',  ( 1.853238653218509890, -9.965882697426144077, 2.398573752920997837 ) ) ;
#13729 = LINE ( 'NONE', #18767, #5814 ) ;
#13730 = VECTOR ( 'NONE', #1991, 1000.000000000000000 ) ;
#13731 = PLANE ( 'NONE',  #54 ) ;
#13732 = VECTOR ( 'NONE', #18637, 1000.000000000000000 ) ;
#13733 = CARTESIAN_POINT ( 'NONE',  ( -1.548630333695928396, -9.114917468222230923, 2.372643865078341019 ) ) ;
#13734 = CARTESIAN_POINT ( 'NONE',  ( -8.496558582316795949, -22.05068747287764452, 0.9999999999999978906 ) ) ;
#13735 = CARTESIAN_POINT ( 'NONE',  ( -1.337453470010121714, -8.364917468222230923, 1.622643865078341907 ) ) ;
#13736 = ORIENTED_EDGE ( 'NONE', *, *, #10378, .F. ) ;
#13737 = CARTESIAN_POINT ( 'NONE',  ( -13.38210008768272630, -19.14144557202113006, 4.745270796715706396 ) ) ;
#13738 = CARTESIAN_POINT ( 'NONE',  ( 13.00209451496117374, 10.00000000000000000, 1.000000000000000000 ) ) ;
#13739 = EDGE_CURVE ( 'NONE', #4438, #15088, #17850, .T. ) ;
#13740 = CARTESIAN_POINT ( 'NONE',  ( 5.309058582316795949, -23.80360840875935935, 1.768074502826626260 ) ) ;
#13741 = CARTESIAN_POINT ( 'NONE',  ( -12.53469141768317741, -20.97900456129164581, 3.136473910504570917 ) ) ;
#13742 = ORIENTED_EDGE ( 'NONE', *, *, #7098, .T. ) ;
#13743 = EDGE_CURVE ( 'NONE', #18598, #20560, #19433, .T. ) ;
#13744 = CARTESIAN_POINT ( 'NONE',  ( 13.37503071710846925, -20.24844878602346299, 4.564052989354591361 ) ) ;
#13745 = CARTESIAN_POINT ( 'NONE',  ( -2.499999999999998668, -19.50000000000000000, 4.000000000000000000 ) ) ;
#13746 = VERTEX_POINT ( 'NONE', #8328 ) ;
#13747 = ORIENTED_EDGE ( 'NONE', *, *, #18871, .F. ) ;
#13748 = LINE ( 'NONE', #7486, #10775 ) ;
#13749 = EDGE_CURVE ( 'NONE', #346, #4104, #384, .T. ) ;
#13750 = ORIENTED_EDGE ( 'NONE', *, *, #195, .T. ) ;
#13751 = CARTESIAN_POINT ( 'NONE',  ( -13.87454419214980739, 4.976981703567351367, 5.131312659523921127 ) ) ;
#13752 = VECTOR ( 'NONE', #14101, 1000.000000000000000 ) ;
#13753 = VERTEX_POINT ( 'NONE', #9996 ) ;
#13754 = CARTESIAN_POINT ( 'NONE',  ( -24.50000000000000000, 0.000000000000000000, 0.000000000000000000 ) ) ;
#13755 = EDGE_CURVE ( 'NONE', #13151, #2226, #16376, .T. ) ;
#13756 = CARTESIAN_POINT ( 'NONE',  ( 10.93924542913430820, 11.64110105645932691, 10.00000000000000000 ) ) ;
#13757 = DIRECTION ( 'NONE',  ( 0.000000000000000000, 0.000000000000000000, 1.000000000000000000 ) ) ;
#13758 = CARTESIAN_POINT ( 'NONE',  ( 1.932703420524435112, -8.381852853175612239, 2.376993210252662969 ) ) ;
#13759 = DIRECTION ( 'NONE',  ( 0.000000000000000000, -1.000000000000000000, 0.000000000000000000 ) ) ;
#13760 = CARTESIAN_POINT ( 'NONE',  ( 12.66204031416134335, -19.12946413485185104, 6.260126454156002218 ) ) ;
#13761 = DIRECTION ( 'NONE',  ( 0.000000000000000000, 0.000000000000000000, 1.000000000000000000 ) ) ;
#13762 = FACE_OUTER_BOUND ( 'NONE', #18110, .T. ) ;
#13763 = CARTESIAN_POINT ( 'NONE',  ( -11.99999999999999822, -18.50000000000000355, 4.000000000000000000 ) ) ;
#13764 = CARTESIAN_POINT ( 'NONE',  ( 4.659691417683178294, -22.67418626127524917, 1.729004561291651809 ) ) ;
#13765 = CARTESIAN_POINT ( 'NONE',  ( 15.50000000000000178, -23.00000000000000711, 4.000000000000000000 ) ) ;
#13766 = CARTESIAN_POINT ( 'NONE',  ( -9.715308582316795949, -23.02099543870833998, 3.136473910504556262 ) ) ;
#13767 = AXIS2_PLACEMENT_3D ( 'NONE', #19736, #7076, #3926 ) ;
#13768 = CARTESIAN_POINT ( 'NONE',  ( -12.34719141768317741, -20.91377862118959285, 1.020995438708345082 ) ) ;
#13769 = EDGE_LOOP ( 'NONE', ( #6266, #12946, #13713, #3843 ) ) ;
#13770 = CARTESIAN_POINT ( 'NONE',  ( 13.11514659413808737, 4.502403003978772134, 5.887634658581065494 ) ) ;
#13771 = CARTESIAN_POINT ( 'NONE',  ( -13.12529397354238192, 5.014845663890295846, 4.916666666666650087 ) ) ;
#13772 = VERTEX_POINT ( 'NONE', #8441 ) ;
#13773 = DIRECTION ( 'NONE',  ( -0.000000000000000000, -0.000000000000000000, -1.000000000000000000 ) ) ;
#13774 = LINE ( 'NONE', #4159, #18026 ) ;
#13775 = ORIENTED_EDGE ( 'NONE', *, *, #19157, .T. ) ;
#13776 = CARTESIAN_POINT ( 'NONE',  ( 1.863950040896528604, -9.995453039732266731, 2.406168007552154098 ) ) ;
#13777 = VERTEX_POINT ( 'NONE', #14808 ) ;
#13778 = ORIENTED_EDGE ( 'NONE', *, *, #13351, .T. ) ;
#13779 = FACE_OUTER_BOUND ( 'NONE', #11302, .T. ) ;
#13780 = EDGE_CURVE ( 'NONE', #10885, #15705, #6862, .T. ) ;
#13781 = CARTESIAN_POINT ( 'NONE',  ( -12.50209451496117197, 11.64110105645932691, 0.000000000000000000 ) ) ;
#13782 = CARTESIAN_POINT ( 'NONE',  ( -1.513434189748285918, -9.864917468222230923, 1.622643865078341907 ) ) ;
#13783 = DIRECTION ( 'NONE',  ( 1.000000000000000000, 0.000000000000000000, 0.000000000000000000 ) ) ;
#13784 = CARTESIAN_POINT ( 'NONE',  ( 21.67243175760212637, 0.000000000000000000, 1.000000000000000000 ) ) ;
#13785 = CARTESIAN_POINT ( 'NONE',  ( 27.44203811574919882, 10.00000000000000000, 1.000000000000000000 ) ) ;
#13786 = CARTESIAN_POINT ( 'NONE',  ( 12.06594141768317741, -23.73192549717336064, 1.696391591240623331 ) ) ;
#13787 = CARTESIAN_POINT ( 'NONE',  ( -12.63819864697926754, -19.58346832754827105, 5.450273968536036406 ) ) ;
#13788 = CARTESIAN_POINT ( 'NONE',  ( -4.940941417683177406, -20.19639159124061933, 1.768074502826635586 ) ) ;
#13789 = ORIENTED_EDGE ( 'NONE', *, *, #9414, .T. ) ;
#13790 = PRODUCT_DEFINITION ( 'UNKNOWN', '', #1696, #18236 ) ;
#13791 = CARTESIAN_POINT ( 'NONE',  ( 20.49999999999998224, -21.99999999999999645, 11.00000000000000178 ) ) ;
#13792 = CARTESIAN_POINT ( 'NONE',  ( -13.60059015675642513, -9.607697083824668027, 6.450359435862663027 ) ) ;
#13793 = CIRCLE ( 'NONE', #4782, 1.499999999999996225 ) ;
#13794 = CARTESIAN_POINT ( 'NONE',  ( 6.059058582316795949, -21.25705176302045274, 4.171265325393551215 ) ) ;
#13795 = DIRECTION ( 'NONE',  ( 0.000000000000000000, 0.000000000000000000, 1.000000000000000000 ) ) ;
#13796 = ORIENTED_EDGE ( 'NONE', *, *, #13257, .T. ) ;
#13797 = VERTEX_POINT ( 'NONE', #15116 ) ;
#13798 = CARTESIAN_POINT ( 'NONE',  ( 13.48548920624593883, -15.42029508461213716, 6.325359435864005064 ) ) ;
#13799 = DIRECTION ( 'NONE',  ( 0.000000000000000000, -1.000000000000000000, 0.000000000000000000 ) ) ;
#13800 = ORIENTED_EDGE ( 'NONE', *, *, #17369, .T. ) ;
#13801 = CARTESIAN_POINT ( 'NONE',  ( 14.50000000000001243, -25.49999999999999645, 4.000000000000000000 ) ) ;
#13802 = ORIENTED_EDGE ( 'NONE', *, *, #19785, .T. ) ;
#13803 = CARTESIAN_POINT ( 'NONE',  ( -8.777808582316792396, -20.27099543870833642, 2.724438792969431589 ) ) ;
#13804 = DIRECTION ( 'NONE',  ( 0.000000000000000000, -0.000000000000000000, 1.000000000000000000 ) ) ;
#13805 = VECTOR ( 'NONE', #3650, 1000.000000000000000 ) ;
#13806 = LINE ( 'NONE', #18942, #14825 ) ;
#13807 = CARTESIAN_POINT ( 'NONE',  ( 2.887553741010006281, -10.84643174835951207, 2.067331322690557638 ) ) ;
#13808 = ADVANCED_FACE ( 'NONE', ( #11769 ), #4031, .T. ) ;
#13809 = LINE ( 'NONE', #8907, #16724 ) ;
#13810 = CARTESIAN_POINT ( 'NONE',  ( -13.09455366754861139, 4.212460211200554916, 5.160171780694988719 ) ) ;
#13811 = LINE ( 'NONE', #2518, #13732 ) ;
#13812 = CARTESIAN_POINT ( 'NONE',  ( -13.48548920624593883, -15.42029508461213716, 6.325359435864005064 ) ) ;
#13813 = DIRECTION ( 'NONE',  ( -0.000000000000000000, -1.000000000000000000, -0.000000000000000000 ) ) ;
#13814 = CARTESIAN_POINT ( 'NONE',  ( 10.09030858231679595, -21.32581373872472597, 1.729004561291657582 ) ) ;
#13815 = EDGE_CURVE ( 'NONE', #5367, #12057, #11970, .T. ) ;
#13816 = CARTESIAN_POINT ( 'NONE',  ( 4.190941417683176518, -23.27327832286946219, 4.701595411283453707 ) ) ;
#13817 = CARTESIAN_POINT ( 'NONE',  ( -8.496558582316794173, -22.05068747287764452, 1.749999999999998446 ) ) ;
#13818 = VERTEX_POINT ( 'NONE', #7384 ) ;
#13819 = CARTESIAN_POINT ( 'NONE',  ( 13.53317008522746434, -11.51241069598931510, 4.909333296715523431 ) ) ;
#13820 = DIRECTION ( 'NONE',  ( 1.000000000000000000, 0.000000000000000000, -0.000000000000000000 ) ) ;
#13821 = ORIENTED_EDGE ( 'NONE', *, *, #5657, .F. ) ;
#13822 = ORIENTED_EDGE ( 'NONE', *, *, #7649, .T. ) ;
#13823 = LINE ( 'NONE', #18650, #8777 ) ;
#13824 = CARTESIAN_POINT ( 'NONE',  ( -12.65650603190776025, -18.65894538865861563, 5.520212342915047365 ) ) ;
#13825 = CARTESIAN_POINT ( 'NONE',  ( -2.583953725994688533, -9.847075946378776479, 2.560676788604062004 ) ) ;
#13826 = CARTESIAN_POINT ( 'NONE',  ( -13.87470586348985258, 4.985146106231644225, 5.033049509202228933 ) ) ;
#13827 = EDGE_CURVE ( 'NONE', #6861, #14893, #16677, .T. ) ;
#13828 = FACE_OUTER_BOUND ( 'NONE', #259, .T. ) ;
#13829 = CARTESIAN_POINT ( 'NONE',  ( -12.62499999999998224, -20.24999999999998934, 4.166666666666636765 ) ) ;
#13830 = PLANE ( 'NONE',  #20395 ) ;
#13831 = CARTESIAN_POINT ( 'NONE',  ( -13.12499999999999645, 5.000000000000047073, 3.999999999999996447 ) ) ;
#13832 = DIRECTION ( 'NONE',  ( -0.000000000000000000, 0.1264857625231113059, -0.9919684228235025047 ) ) ;
#13833 = CARTESIAN_POINT ( 'NONE',  ( -9.059058582316795949, -20.19639159124062999, 5.231925497173373074 ) ) ;
#13834 = CARTESIAN_POINT ( 'NONE',  ( -2.780192134145684779, -10.08406280675441735, 1.871539748636713130 ) ) ;
#13835 = EDGE_CURVE ( 'NONE', #4154, #8135, #13439, .T. ) ;
#13836 = ORIENTED_EDGE ( 'NONE', *, *, #16549, .T. ) ;
#13837 = ADVANCED_FACE ( 'NONE', ( #3825 ), #10205, .T. ) ;
#13838 = CARTESIAN_POINT ( 'NONE',  ( -13.84497512400090891, 4.233743762047977199, 5.032110966142367303 ) ) ;
#13839 = CARTESIAN_POINT ( 'NONE',  ( 0.000000000000000000, 9.000000000000001776, 1.000000000000000000 ) ) ;
#13840 = CARTESIAN_POINT ( 'NONE',  ( 5.121558582316795061, -24.50000000000000000, 3.550687472877651629 ) ) ;
#13841 = CARTESIAN_POINT ( 'NONE',  ( -8.690941417683177406, -22.74294823697955081, 4.171265325393542334 ) ) ;
#13842 = EDGE_LOOP ( 'NONE', ( #3901, #5284, #1645, #11566 ) ) ;
#13843 = CARTESIAN_POINT ( 'NONE',  ( 13.37499964066394043, -21.00001814646822496, 4.442866346476199269 ) ) ;
#13844 = CARTESIAN_POINT ( 'NONE',  ( 15.36404127825609400, 0.000000000000000000, 1.000000000000000000 ) ) ;
#13845 = EDGE_LOOP ( 'NONE', ( #2384, #221, #19199, #13336 ) ) ;
#13846 = EDGE_CURVE ( 'NONE', #965, #19224, #16572, .T. ) ;
#13847 = ORIENTED_EDGE ( 'NONE', *, *, #17959, .T. ) ;
#13848 = DIRECTION ( 'NONE',  ( 0.000000000000000000, 0.000000000000000000, -1.000000000000000000 ) ) ;
#13849 = VERTEX_POINT ( 'NONE', #4234 ) ;
#13850 = CARTESIAN_POINT ( 'NONE',  ( -13.77789853026076550, 0.09637577819625635367, 5.909013032956687006 ) ) ;
#13851 = CARTESIAN_POINT ( 'NONE',  ( 2.203959450683124377, -9.262433282444222371, 2.410528873095051594 ) ) ;
#13852 = ORIENTED_EDGE ( 'NONE', *, *, #15273, .F. ) ;
#13853 = FACE_OUTER_BOUND ( 'NONE', #10094, .T. ) ;
#13854 = DIRECTION ( 'NONE',  ( 0.000000000000000000, 1.000000000000000000, -0.000000000000000000 ) ) ;
#13855 = ADVANCED_FACE ( 'NONE', ( #16988, #15216 ), #12181, .F. ) ;
#13856 = EDGE_CURVE ( 'NONE', #1111, #17042, #3924, .T. ) ;
#13857 = CARTESIAN_POINT ( 'NONE',  ( 0.000000000000000000, 0.000000000000000000, 1.000000000000000000 ) ) ;
#13858 = CARTESIAN_POINT ( 'NONE',  ( 3.462011766956747394, -14.92507028461178287, 3.114807177791267812 ) ) ;
#13859 = DIRECTION ( 'NONE',  ( 0.1351665943404306014, -0.9596796555888911229, 0.2464649070825229160 ) ) ;
#13860 = VECTOR ( 'NONE', #4485, 1000.000000000000000 ) ;
#13861 = CARTESIAN_POINT ( 'NONE',  ( 13.10012427866737639, 3.743776072700027324, 6.001983176248468332 ) ) ;
#13862 = LINE ( 'NONE', #5724, #9288 ) ;
#13863 = CARTESIAN_POINT ( 'NONE',  ( -24.79469207716615031, 4.999999999999999112, 1.000000000000000000 ) ) ;
#13864 = DIRECTION ( 'NONE',  ( -0.000000000000000000, 0.000000000000000000, -1.000000000000000000 ) ) ;
#13865 = CIRCLE ( 'NONE', #3511, 0.2500000000000002220 ) ;
#13866 = VECTOR ( 'NONE', #9189, 1000.000000000000000 ) ;
#13867 = CARTESIAN_POINT ( 'NONE',  ( 7.284691417683176518, -23.02099543870834353, 3.863526089495429972 ) ) ;
#13868 = CARTESIAN_POINT ( 'NONE',  ( -12.69247507894198712, -16.84250851341299082, 5.559274842915185033 ) ) ;
#13869 = CARTESIAN_POINT ( 'NONE',  ( -8.684058582316795949, -21.32873467460644079, 2.757051763020455404 ) ) ;
#13870 = CARTESIAN_POINT ( 'NONE',  ( -9.909691417683175629, -21.01515356694492098, 6.020995438708349745 ) ) ;
#13871 = ORIENTED_EDGE ( 'NONE', *, *, #18576, .T. ) ;
#13872 = CARTESIAN_POINT ( 'NONE',  ( 13.12529397354238192, 5.014845663890295846, 3.666666666666500873 ) ) ;
#13873 = CARTESIAN_POINT ( 'NONE',  ( -13.10624331898488037, 4.052787608736739600, 6.006964772046813117 ) ) ;
#13874 = ORIENTED_EDGE ( 'NONE', *, *, #14003, .F. ) ;
#13875 = CARTESIAN_POINT ( 'NONE',  ( -6.313547257480587760, 11.64110105645932691, 0.000000000000000000 ) ) ;
#13876 = ORIENTED_EDGE ( 'NONE', *, *, #6264, .F. ) ;
#13877 = CARTESIAN_POINT ( 'NONE',  ( 0.000000000000000000, -9.864917468222230923, 2.372643865078341019 ) ) ;
#13878 = EDGE_LOOP ( 'NONE', ( #15556, #5626, #15955, #7131 ) ) ;
#13879 = LINE ( 'NONE', #20185, #18345 ) ;
#13880 = DIRECTION ( 'NONE',  ( 1.000000000000000000, 0.000000000000000000, 0.000000000000000000 ) ) ;
#13881 = EDGE_CURVE ( 'NONE', #4496, #15932, #18370, .T. ) ;
#13882 = EDGE_CURVE ( 'NONE', #8244, #1149, #13748, .T. ) ;
#13883 = CARTESIAN_POINT ( 'NONE',  ( -2.022757268986824730, -10.07035769906783784, 1.675405020440470238 ) ) ;
#13884 = CARTESIAN_POINT ( 'NONE',  ( -27.94203811574920948, 16.00000000000000000, 1.000000000000000000 ) ) ;
#13885 = DIRECTION ( 'NONE',  ( -1.000000000000000000, -2.312964634635731617E-15, 0.000000000000000000 ) ) ;
#13886 = LINE ( 'NONE', #20287, #3680 ) ;
#13887 = CARTESIAN_POINT ( 'NONE',  ( 5.965308582316795949, -19.47900456129164937, 4.484846433055089676 ) ) ;
#13888 = CARTESIAN_POINT ( 'NONE',  ( -12.62888984277510218, -20.05356293986039873, 5.111704976569332537 ) ) ;
#13889 = CARTESIAN_POINT ( 'NONE',  ( -8.409691417683177406, -21.32581373872474373, 5.270995438708348857 ) ) ;
#13890 = ORIENTED_EDGE ( 'NONE', *, *, #7828, .F. ) ;
#13891 = FACE_OUTER_BOUND ( 'NONE', #11059, .T. ) ;
#13892 = PLANE ( 'NONE',  #9745 ) ;
#13893 = CARTESIAN_POINT ( 'NONE',  ( -13.87824226375436965, 4.413734319597230282, 6.694665752684481497 ) ) ;
#13894 = VERTEX_POINT ( 'NONE', #16788 ) ;
#13895 = EDGE_CURVE ( 'NONE', #175, #16502, #687, .T. ) ;
#13896 = CARTESIAN_POINT ( 'NONE',  ( 9.715308582316794173, -23.77099543870833998, 2.825813738724734847 ) ) ;
#13897 = CARTESIAN_POINT ( 'NONE',  ( 0.000000000000000000, 4.999999999999999112, 1.000000000000000000 ) ) ;
#13898 = ORIENTED_EDGE ( 'NONE', *, *, #5507, .F. ) ;
#13899 = VERTEX_POINT ( 'NONE', #8943 ) ;
#13900 = CARTESIAN_POINT ( 'NONE',  ( 13.37543017851028893, -20.97827598523083026, 4.780017688621249761 ) ) ;
#13901 = DIRECTION ( 'NONE',  ( -0.000000000000000000, -0.000000000000000000, -1.000000000000000000 ) ) ;
#13902 = VERTEX_POINT ( 'NONE', #2666 ) ;
#13903 = DIRECTION ( 'NONE',  ( 1.000000000000000000, 0.000000000000000000, 0.000000000000000000 ) ) ;
#13904 = ORIENTED_EDGE ( 'NONE', *, *, #19330, .F. ) ;
#13905 = CARTESIAN_POINT ( 'NONE',  ( -12.99655858231679417, -22.05068747287764452, 1.749999999999998446 ) ) ;
#13906 = DIRECTION ( 'NONE',  ( 0.000000000000000000, 0.000000000000000000, 1.000000000000000000 ) ) ;
#13907 = DIRECTION ( 'NONE',  ( -0.000000000000000000, 0.000000000000000000, 1.000000000000000000 ) ) ;
#13908 = CARTESIAN_POINT ( 'NONE',  ( 2.012076196476103362, -9.160103213191565175, 1.634248467062433541 ) ) ;
#13909 = DIRECTION ( 'NONE',  ( 0.000000000000000000, 1.000000000000000000, -0.000000000000000000 ) ) ;
#13910 = CARTESIAN_POINT ( 'NONE',  ( -13.09553549038190567, 4.262042264285192950, 5.042530537310905281 ) ) ;
#13911 = CARTESIAN_POINT ( 'NONE',  ( 12.05905858231679417, -20.72672167713054137, 4.701595411283463477 ) ) ;
#13912 = CARTESIAN_POINT ( 'NONE',  ( -13.39169349927020569, -20.15697828685464188, 6.009339318877812808 ) ) ;
#13913 = CARTESIAN_POINT ( 'NONE',  ( 11.99999999999999822, -17.50000000000000000, 4.000000000000000000 ) ) ;
#13914 = CARTESIAN_POINT ( 'NONE',  ( 4.746558582316795061, -21.94931252712234127, 4.499999999999999112 ) ) ;
#13915 = VECTOR ( 'NONE', #12441, 1000.000000000000000 ) ;
#13916 = CARTESIAN_POINT ( 'NONE',  ( 9.909691417683175629, -21.63647391050456648, 4.520995438708348857 ) ) ;
#13917 = CARTESIAN_POINT ( 'NONE',  ( -7.277808582316794173, -20.27099543870833642, 2.724438792969431589 ) ) ;
#13918 = ORIENTED_EDGE ( 'NONE', *, *, #18596, .T. ) ;
#13919 = CARTESIAN_POINT ( 'NONE',  ( 13.39888564296547635, -18.29377503024027263, 4.763499963382565205 ) ) ;
#13920 = AXIS2_PLACEMENT_3D ( 'NONE', #19607, #18343, #11638 ) ;
#13921 = CARTESIAN_POINT ( 'NONE',  ( -2.747777887823422471, -9.906471667804277459, 1.825930796414880763 ) ) ;
#13922 = EDGE_LOOP ( 'NONE', ( #12591, #2804, #14044, #7843, #5472, #9577 ) ) ;
#13923 = ADVANCED_FACE ( 'NONE', ( #9054 ), #11871, .T. ) ;
#13924 = ORIENTED_EDGE ( 'NONE', *, *, #18743, .F. ) ;
#13925 = LINE ( 'NONE', #869, #15115 ) ;
#13926 = CARTESIAN_POINT ( 'NONE',  ( -13.10557919622060652, 4.019249409169220577, 6.007898877577752650 ) ) ;
#13927 = LINE ( 'NONE', #13521, #5293 ) ;
#13928 = CARTESIAN_POINT ( 'NONE',  ( -13.81626551376501588, 2.033908445126689557, 5.950679699622869911 ) ) ;
#13929 = LINE ( 'NONE', #20026, #20692 ) ;
#13930 = CARTESIAN_POINT ( 'NONE',  ( -20.00000000000000000, -6.000000000000000000, 1.000000000000000000 ) ) ;
#13931 = DIRECTION ( 'NONE',  ( -1.000000000000000000, -0.000000000000000000, -0.000000000000000000 ) ) ;
#13932 = FACE_OUTER_BOUND ( 'NONE', #12750, .T. ) ;
#13933 = LINE ( 'NONE', #15202, #11316 ) ;
#13934 = CARTESIAN_POINT ( 'NONE',  ( -10.37155858231679595, -19.49999999999998934, 3.449312527122348371 ) ) ;
#13935 = CARTESIAN_POINT ( 'NONE',  ( -1.819865260185086875, -9.122006307963404836, 1.624464420737683046 ) ) ;
#13936 = ORIENTED_EDGE ( 'NONE', *, *, #16387, .F. ) ;
#13937 = VECTOR ( 'NONE', #18289, 1000.000000000000000 ) ;
#13938 = CARTESIAN_POINT ( 'NONE',  ( -13.83973345681288158, 3.969039569021246550, 5.242263935944164288 ) ) ;
#13939 = FACE_OUTER_BOUND ( 'NONE', #15623, .T. ) ;
#13940 = CARTESIAN_POINT ( 'NONE',  ( 12.34719141768317741, -20.91377862118959285, 1.020995438708345082 ) ) ;
#13941 = CARTESIAN_POINT ( 'NONE',  ( -3.974842109207560537, -21.92432777746334693, 4.506404853634142782 ) ) ;
#13942 = ORIENTED_EDGE ( 'NONE', *, *, #19738, .T. ) ;
#13943 = CARTESIAN_POINT ( 'NONE',  ( 13.85980676119184629, 4.232741440188380722, 5.965367510457697975 ) ) ;
#13944 = LINE ( 'NONE', #6118, #8714 ) ;
#13945 = VERTEX_POINT ( 'NONE', #13541 ) ;
#13946 = ORIENTED_EDGE ( 'NONE', *, *, #10196, .T. ) ;
#13947 = CARTESIAN_POINT ( 'NONE',  ( -26.04469207716614676, 4.999999999999999112, 1.000000000000000000 ) ) ;
#13948 = EDGE_CURVE ( 'NONE', #5550, #1363, #792, .T. ) ;
#13949 = VERTEX_POINT ( 'NONE', #2455 ) ;
#13950 = PLANE ( 'NONE',  #17444 ) ;
#13951 = CARTESIAN_POINT ( 'NONE',  ( -0.000000000000000000, 10.00000000000000000, 0.000000000000000000 ) ) ;
#13952 = EDGE_CURVE ( 'NONE', #2483, #13360, #4134, .T. ) ;
#13953 = EDGE_CURVE ( 'NONE', #19964, #8687, #996, .T. ) ;
#13954 = EDGE_LOOP ( 'NONE', ( #18448, #16081, #18856, #10979 ) ) ;
#13955 = LINE ( 'NONE', #18790, #20567 ) ;
#13956 = PLANE ( 'NONE',  #16035 ) ;
#13957 = AXIS2_PLACEMENT_3D ( 'NONE', #5762, #100, #20715 ) ;
#13958 = CARTESIAN_POINT ( 'NONE',  ( 11.00000000000000000, -19.49999999999999645, 5.000000000000000000 ) ) ;
#13959 = CARTESIAN_POINT ( 'NONE',  ( 2.309828811027716977, -9.292785183284841821, 1.668323847571005603 ) ) ;
#13960 = DIRECTION ( 'NONE',  ( 3.469446951953611033E-15, -1.000000000000000000, 0.000000000000000000 ) ) ;
#13961 = DIRECTION ( 'NONE',  ( 1.000000000000000000, 0.000000000000000000, 0.000000000000000000 ) ) ;
#13962 = CYLINDRICAL_SURFACE ( 'NONE', #18990, 2.999999999999999112 ) ;
#13963 = CARTESIAN_POINT ( 'NONE',  ( -2.061130159782011972, 9.000000000000001776, 0.000000000000000000 ) ) ;
#13964 = CARTESIAN_POINT ( 'NONE',  ( -14.49999999999998579, -19.49999999999999645, 4.000000000000000000 ) ) ;
#13965 = VECTOR ( 'NONE', #5940, 1000.000000000000000 ) ;
#13966 = CARTESIAN_POINT ( 'NONE',  ( 4.565941417683176518, -22.67126532539353789, 2.757051763020445634 ) ) ;
#13967 = CARTESIAN_POINT ( 'NONE',  ( -13.12529397354238192, 5.014845663890295846, 4.583333333333296622 ) ) ;
#13968 = CARTESIAN_POINT ( 'NONE',  ( -12.24655858231679595, -21.94931252712234127, 4.499999999999999112 ) ) ;
#13969 = CARTESIAN_POINT ( 'NONE',  ( -9.253441417683177406, -21.94931252712233061, 0.9999999999999978906 ) ) ;
#13970 = VECTOR ( 'NONE', #19236, 1000.000000000000000 ) ;
#13971 = ORIENTED_EDGE ( 'NONE', *, *, #20088, .F. ) ;
#13972 = CARTESIAN_POINT ( 'NONE',  ( 13.09560269887985307, 4.265436293439658577, 4.973800642626965640 ) ) ;
#13973 = DIRECTION ( 'NONE',  ( 1.000000000000000000, -0.000000000000000000, 0.000000000000000000 ) ) ;
#13974 = EDGE_LOOP ( 'NONE', ( #3697, #840, #5938, #1159 ) ) ;
#13975 = CARTESIAN_POINT ( 'NONE',  ( 28.94203811574921659, 16.00000000000000000, 1.000000000000000000 ) ) ;
#13976 = EDGE_CURVE ( 'NONE', #20490, #5162, #9155, .T. ) ;
#13977 = ORIENTED_EDGE ( 'NONE', *, *, #9541, .T. ) ;
#13978 = CARTESIAN_POINT ( 'NONE',  ( 1.853238653218509890, -9.965882697426144077, 2.398573752920997837 ) ) ;
#13979 = ORIENTED_EDGE ( 'NONE', *, *, #1308, .F. ) ;
#13980 = PLANE ( 'NONE',  #16992 ) ;
#13981 = CARTESIAN_POINT ( 'NONE',  ( 17.30017143803810242, 4.999999999999999112, 0.000000000000000000 ) ) ;
#13982 = VECTOR ( 'NONE', #6818, 1000.000000000000000 ) ;
#13983 = CARTESIAN_POINT ( 'NONE',  ( -1.963707630584672570, -9.980492102769451535, 1.652325740065381909 ) ) ;
#13984 = PLANE ( 'NONE',  #15322 ) ;
#13985 = LINE ( 'NONE', #12525, #6967 ) ;
#13986 = AXIS2_PLACEMENT_3D ( 'NONE', #14837, #19656, #16506 ) ;
#13987 = ADVANCED_FACE ( 'NONE', ( #9742 ), #9353, .T. ) ;
#13988 = CARTESIAN_POINT ( 'NONE',  ( 8.597191417683177406, -23.08622137881040359, 5.979004561291654696 ) ) ;
#13989 = CARTESIAN_POINT ( 'NONE',  ( -13.12529397354238192, 5.014845663890295846, 3.666666666666500873 ) ) ;
#13990 = CARTESIAN_POINT ( 'NONE',  ( -8.222191417683175629, -20.27099543870833998, 4.275561207030583510 ) ) ;
#13991 = VERTEX_POINT ( 'NONE', #16014 ) ;
#13992 = CARTESIAN_POINT ( 'NONE',  ( 8.215308582316792396, -23.77099543870833998, 2.825813738724734847 ) ) ;
#13993 = LINE ( 'NONE', #18929, #727 ) ;
#13994 = CARTESIAN_POINT ( 'NONE',  ( -12.63178515739782348, -20.65734955141111584, 5.567013446834313761 ) ) ;
#13995 = AXIS2_PLACEMENT_3D ( 'NONE', #4351, #10736, #4554 ) ;
#13996 = VECTOR ( 'NONE', #11667, 1000.000000000000000 ) ;
#13997 = VERTEX_POINT ( 'NONE', #10726 ) ;
#13998 = CARTESIAN_POINT ( 'NONE',  ( 7.371558582316794173, -20.24999999999999289, 3.449312527122348371 ) ) ;
#13999 = EDGE_CURVE ( 'NONE', #2481, #20051, #12492, .T. ) ;
#14000 = DIRECTION ( 'NONE',  ( 1.000000000000000000, 0.000000000000000000, -0.000000000000000000 ) ) ;
#14001 = AXIS2_PLACEMENT_3D ( 'NONE', #11793, #11685, #18183 ) ;
#14002 = ORIENTED_EDGE ( 'NONE', *, *, #6868, .T. ) ;
#14003 = EDGE_CURVE ( 'NONE', #15372, #3140, #18884, .T. ) ;
#14004 = ORIENTED_EDGE ( 'NONE', *, *, #20615, .T. ) ;
#14005 = CARTESIAN_POINT ( 'NONE',  ( 13.37671366598624800, -20.91345986769124465, 5.053911344471881506 ) ) ;
#14006 = LINE ( 'NONE', #13690, #20275 ) ;
#14007 = ORIENTED_EDGE ( 'NONE', *, *, #10425, .F. ) ;
#14008 = CARTESIAN_POINT ( 'NONE',  ( -8.376396343307449754, 10.00000000000000000, 1.000000000000000000 ) ) ;
#14009 = ORIENTED_EDGE ( 'NONE', *, *, #8139, .F. ) ;
#14010 = DIRECTION ( 'NONE',  ( -0.000000000000000000, -0.000000000000000000, -1.000000000000000000 ) ) ;
#14011 = LINE ( 'NONE', #9209, #15594 ) ;
#14012 = CARTESIAN_POINT ( 'NONE',  ( 2.693754455098655409, -10.04853567022903782, 2.237415670251142519 ) ) ;
#14013 = CARTESIAN_POINT ( 'NONE',  ( 0.000000000000000000, -8.364917468222230923, 1.622643865078341241 ) ) ;
#14014 = EDGE_CURVE ( 'NONE', #7416, #2967, #4342, .T. ) ;
#14015 =( REPRESENTATION_RELATIONSHIP ('NONE','NONE', #1880, #14706 ) REPRESENTATION_RELATIONSHIP_WITH_TRANSFORMATION ( #818 )SHAPE_REPRESENTATION_RELATIONSHIP( ) );
#14016 = CARTESIAN_POINT ( 'NONE',  ( -14.49999999999998579, -24.49999999999999289, 4.000000000000000000 ) ) ;
#14017 = CARTESIAN_POINT ( 'NONE',  ( -13.08080186171710224, 3.517994016715657146, 5.247095106674282583 ) ) ;
#14018 = AXIS2_PLACEMENT_3D ( 'NONE', #14269, #17519, #20578 ) ;
#14019 = CARTESIAN_POINT ( 'NONE',  ( 6.152808582316793284, -21.22443879296942626, 5.229004561291659137 ) ) ;
#14020 = CARTESIAN_POINT ( 'NONE',  ( -12.67103257592000176, -18.67535491604046172, 6.269892079155907183 ) ) ;
#14021 = VECTOR ( 'NONE', #9929, 1000.000000000000000 ) ;
#14022 = CARTESIAN_POINT ( 'NONE',  ( 0.000000000000000000, 0.000000000000000000, 1.000000000000000000 ) ) ;
#14023 = CARTESIAN_POINT ( 'NONE',  ( 4.840308582316795061, -22.36352608949544418, 4.520995438708343528 ) ) ;
#14024 = CARTESIAN_POINT ( 'NONE',  ( 9.347191417683177406, -21.53509896474923835, 2.520995438708346192 ) ) ;
#14025 = CARTESIAN_POINT ( 'NONE',  ( -6.340308582316793284, -22.67418626127525982, 5.270995438708342640 ) ) ;
#14026 = VERTEX_POINT ( 'NONE', #5908 ) ;
#14027 = CARTESIAN_POINT ( 'NONE',  ( 13.38929389708972195, -18.77815819697223887, 4.753083296715700179 ) ) ;
#14028 = CARTESIAN_POINT ( 'NONE',  ( -0.5631383031621635116, -9.114917468222230923, 1.622643865078341463 ) ) ;
#14029 = EDGE_LOOP ( 'NONE', ( #11185, #15649 ) ) ;
#14030 =( BOUNDED_CURVE ( )  B_SPLINE_CURVE ( 3, ( #17359, #7849, #15791, #5870 ),
 .UNSPECIFIED., .F., .F. ) 
 B_SPLINE_CURVE_WITH_KNOTS ( ( 4, 4 ),
 ( 0.001187255941418635012, 0.002344578398797381343 ),
 .UNSPECIFIED. ) 
 CURVE ( )  GEOMETRIC_REPRESENTATION_ITEM ( )  RATIONAL_B_SPLINE_CURVE ( ( 0.9619191252709787809, 0.3335846922424358096, 0.3462783171521095493, 1.000000000000000000 ) ) 
 REPRESENTATION_ITEM ( '' )  );
#14031 = ORIENTED_EDGE ( 'NONE', *, *, #4034, .F. ) ;
#14032 = LINE ( 'NONE', #15598, #19476 ) ;
#14033 = CIRCLE ( 'NONE', #18398, 10.00000000000000000 ) ;
#14034 = CARTESIAN_POINT ( 'NONE',  ( -12.69247507894198712, -16.84250851341299082, 5.559274842915185033 ) ) ;
#14035 = CARTESIAN_POINT ( 'NONE',  ( -1.717920576997000737, -9.114924032904250240, 2.372645551019823884 ) ) ;
#14036 = CARTESIAN_POINT ( 'NONE',  ( -13.86470821076586368, 4.480264643675554659, 5.874551681240599343 ) ) ;
#14037 = EDGE_CURVE ( 'NONE', #411, #6312, #19376, .T. ) ;
#14038 = DIRECTION ( 'NONE',  ( 1.000000000000000000, 0.000000000000000000, -0.000000000000000000 ) ) ;
#14039 = CARTESIAN_POINT ( 'NONE',  ( 27.00000000000000000, 0.000000000000000000, 0.000000000000000000 ) ) ;
#14040 = LINE ( 'NONE', #12476, #19394 ) ;
#14041 = DIRECTION ( 'NONE',  ( 0.000000000000000000, 0.000000000000000000, 1.000000000000000000 ) ) ;
#14042 = CARTESIAN_POINT ( 'NONE',  ( -11.30905858231679595, -23.80360840875935935, 1.768074502826626260 ) ) ;
#14043 = CARTESIAN_POINT ( 'NONE',  ( -3.347120161770001268, -14.10934257735911146, 2.905312006771028077 ) ) ;
#14044 = ORIENTED_EDGE ( 'NONE', *, *, #11822, .F. ) ;
#14045 = CARTESIAN_POINT ( 'NONE',  ( -13.84090061271218985, 4.027980941966571748, 5.240332426532912535 ) ) ;
#14046 = DIRECTION ( 'NONE',  ( 0.000000000000000000, -0.000000000000000000, 1.000000000000000000 ) ) ;
#14047 = VECTOR ( 'NONE', #16244, 1000.000000000000000 ) ;
#14048 = CARTESIAN_POINT ( 'NONE',  ( 9.815941417683177406, -20.26807450282663225, 5.303608408759377113 ) ) ;
#14049 = CARTESIAN_POINT ( 'NONE',  ( -4.003441417683175629, -22.05068747287766229, 4.499999999999999112 ) ) ;
#14050 = ORIENTED_EDGE ( 'NONE', *, *, #12096, .F. ) ;
#14051 = VECTOR ( 'NONE', #8088, 1000.000000000000000 ) ;
#14052 = CARTESIAN_POINT ( 'NONE',  ( 13.41115317570721110, -19.17426462678482579, 6.244630269197427808 ) ) ;
#14053 = CARTESIAN_POINT ( 'NONE',  ( 12.62499999999998224, -20.24999999999991829, 4.333333333333343695 ) ) ;
#14054 = VERTEX_POINT ( 'NONE', #5031 ) ;
#14055 = ORIENTED_EDGE ( 'NONE', *, *, #11197, .T. ) ;
#14056 = CARTESIAN_POINT ( 'NONE',  ( -5.000000000000000000, -12.50000000000000000, 1.000000000000000000 ) ) ;
#14057 = VERTEX_POINT ( 'NONE', #7584 ) ;
#14058 = CARTESIAN_POINT ( 'NONE',  ( -13.40621837757088564, -18.67347193267085714, 5.505367199623145247 ) ) ;
#14059 = CARTESIAN_POINT ( 'NONE',  ( 1.126276606324276619, -9.114917468222230923, 2.372643865078341019 ) ) ;
#14060 = VERTEX_POINT ( 'NONE', #124 ) ;
#14061 = CARTESIAN_POINT ( 'NONE',  ( -3.944195004867013132, -21.63820656525943775, 5.112513974992745958 ) ) ;
#14062 = DIRECTION ( 'NONE',  ( 0.7071067811865474617, -0.000000000000000000, -0.7071067811865474617 ) ) ;
#14063 = VECTOR ( 'NONE', #11834, 1000.000000000000000 ) ;
#14064 = VECTOR ( 'NONE', #14496, 1000.000000000000000 ) ;
#14065 = LINE ( 'NONE', #18792, #1971 ) ;
#14066 = CARTESIAN_POINT ( 'NONE',  ( 2.682825141213236009, -9.727160171598653093, 1.779880022082258373 ) ) ;
#14067 = PLANE ( 'NONE',  #1475 ) ;
#14068 = CARTESIAN_POINT ( 'NONE',  ( 13.12529397354238192, 5.014845663890295846, 4.833333333333344584 ) ) ;
#14069 = EDGE_CURVE ( 'NONE', #2663, #12837, #6605, .T. ) ;
#14070 = LINE ( 'NONE', #1123, #3615 ) ;
#14071 = CARTESIAN_POINT ( 'NONE',  ( 20.50349085826861995, 11.64110105645932691, 10.00000000000000000 ) ) ;
#14072 = LINE ( 'NONE', #13651, #1028 ) ;
#14073 = CARTESIAN_POINT ( 'NONE',  ( 12.90280858231679595, -22.46490103525074034, 2.520995438708341307 ) ) ;
#14074 = CARTESIAN_POINT ( 'NONE',  ( -12.62499999998404299, -19.49999999996810729, 2.793053905886972998 ) ) ;
#14075 = CARTESIAN_POINT ( 'NONE',  ( -12.71530858231679417, -23.02099543870833998, 3.136473910504556262 ) ) ;
#14076 = CARTESIAN_POINT ( 'NONE',  ( -6.440941417683175629, -20.19639159124061933, 1.768074502826635586 ) ) ;
#14077 = ORIENTED_EDGE ( 'NONE', *, *, #1492, .F. ) ;
#14078 = ADVANCED_FACE ( 'NONE', ( #7687 ), #11304, .T. ) ;
#14079 = CARTESIAN_POINT ( 'NONE',  ( 13.09106898171683930, 4.036483576700608644, 5.256123545019964816 ) ) ;
#14080 = CARTESIAN_POINT ( 'NONE',  ( -20.92243175760212637, 4.999999999999999112, 1.000000000000000000 ) ) ;
#14081 = ORIENTED_EDGE ( 'NONE', *, *, #5397, .F. ) ;
#14082 = EDGE_CURVE ( 'NONE', #6097, #13688, #14547, .T. ) ;
#14083 = VECTOR ( 'NONE', #5951, 1000.000000000000000 ) ;
#14084 = DIRECTION ( 'NONE',  ( -0.000000000000000000, 1.000000000000000000, -0.000000000000000000 ) ) ;
#14085 = EDGE_LOOP ( 'NONE', ( #13668, #6236, #4080, #15051 ) ) ;
#14086 = CARTESIAN_POINT ( 'NONE',  ( 2.659620708751979645, -10.38426118526329489, 2.698636689302993830 ) ) ;
#14087 = VERTEX_POINT ( 'NONE', #12280 ) ;
#14088 = CARTESIAN_POINT ( 'NONE',  ( -11.00000000000000000, -19.49999999999999645, 4.000000000000000000 ) ) ;
#14089 = DIRECTION ( 'NONE',  ( 0.000000000000000000, 0.000000000000000000, 1.000000000000000000 ) ) ;
#14090 = CARTESIAN_POINT ( 'NONE',  ( -1.126276606324276619, -9.864917468222230923, 1.622643865078341907 ) ) ;
#14091 = CARTESIAN_POINT ( 'NONE',  ( -11.24178095869206828, 4.999999999999999112, 0.000000000000000000 ) ) ;
#14092 = CARTESIAN_POINT ( 'NONE',  ( -9.305650798910056309, 0.000000000000000000, 1.000000000000000000 ) ) ;
#14093 = VECTOR ( 'NONE', #13138, 1000.000000000000000 ) ;
#14094 = ADVANCED_FACE ( 'NONE', ( #3361 ), #219, .T. ) ;
#14095 = CARTESIAN_POINT ( 'NONE',  ( -3.999999999999999112, -7.500000000000047073, 2.000000000000000000 ) ) ;
#14096 = CARTESIAN_POINT ( 'NONE',  ( 12.53469141768317741, -20.22900456129164581, 2.825813738724747726 ) ) ;
#14097 = LINE ( 'NONE', #20397, #7870 ) ;
#14098 = CARTESIAN_POINT ( 'NONE',  ( -12.25344141768317741, -21.94931252712233061, 1.749999999999998446 ) ) ;
#14099 = EDGE_LOOP ( 'NONE', ( #5203, #18447, #7840, #6524 ) ) ;
#14100 = CARTESIAN_POINT ( 'NONE',  ( 5.871558582316794173, -20.24999999999999289, 3.449312527122348371 ) ) ;
#14101 = DIRECTION ( 'NONE',  ( -0.000000000000000000, -0.000000000000000000, -1.000000000000000000 ) ) ;
#14102 = CARTESIAN_POINT ( 'NONE',  ( -13.90439735423812273, 5.734566389025032684, 4.583333333333295734 ) ) ;
#14103 = ORIENTED_EDGE ( 'NONE', *, *, #1584, .F. ) ;
#14104 = AXIS2_PLACEMENT_3D ( 'NONE', #2299, #11716, #743 ) ;
#14105 = CARTESIAN_POINT ( 'NONE',  ( 5.402808582316794173, -22.77556120703056308, 1.770995438708339975 ) ) ;
#14106 = CARTESIAN_POINT ( 'NONE',  ( -14.99999999999999645, -30.00000000000000711, 1.000000000000000000 ) ) ;
#14107 = ORIENTED_EDGE ( 'NONE', *, *, #13827, .F. ) ;
#14108 = CARTESIAN_POINT ( 'NONE',  ( -14.56494360078803396, 11.64110105645932691, 10.00000000000000000 ) ) ;
#14109 = SHAPE_REPRESENTATION_RELATIONSHIP ( 'NONE' , 'NONE' ,  #537, #15532 ) ;
#14110 = EDGE_LOOP ( 'NONE', ( #1161, #6477, #1656, #19438 ) ) ;
#14111 = EDGE_CURVE ( 'NONE', #1942, #7441, #17798, .T. ) ;
#14112 = VECTOR ( 'NONE', #12256, 1000.000000000000000 ) ;
#14113 = DIRECTION ( 'NONE',  ( 1.000000000000000000, -3.469446951953491127E-15, 0.000000000000000000 ) ) ;
#14114 = VERTEX_POINT ( 'NONE', #14056 ) ;
#14115 = CARTESIAN_POINT ( 'NONE',  ( -11.40280858231679417, -22.77556120703056308, 1.770995438708339975 ) ) ;
#14116 = CARTESIAN_POINT ( 'NONE',  ( 7.619520639128047002, 4.999999999999999112, 1.000000000000000000 ) ) ;
#14117 = FACE_OUTER_BOUND ( 'NONE', #20564, .T. ) ;
#14118 = CARTESIAN_POINT ( 'NONE',  ( 1.337453470010121714, -8.364917468222230923, 1.622643865078341907 ) ) ;
#14119 = EDGE_CURVE ( 'NONE', #2052, #9026, #1209, .T. ) ;
#14120 = ADVANCED_FACE ( 'NONE', ( #20250 ), #12389, .T. ) ;
#14121 = DIRECTION ( 'NONE',  ( 1.000000000000000000, 0.000000000000000000, 0.000000000000000000 ) ) ;
#14122 = CARTESIAN_POINT ( 'NONE',  ( -13.09560264576187905, 4.265433610975056133, 4.166666666666765551 ) ) ;
#14123 = CARTESIAN_POINT ( 'NONE',  ( 5.309058582316794173, -23.27327832286945153, 2.298404588716537411 ) ) ;
#14124 = CARTESIAN_POINT ( 'NONE',  ( -12.62499999999998401, -20.99999999999998934, 2.439580858552613751 ) ) ;
#14125 = VECTOR ( 'NONE', #7692, 1000.000000000000000 ) ;
#14126 = CARTESIAN_POINT ( 'NONE',  ( -13.12529397354238192, 5.014845663890297622, 3.999999999999981792 ) ) ;
#14127 = CARTESIAN_POINT ( 'NONE',  ( 7.652808582316795061, -21.22443879296942626, 5.229004561291659137 ) ) ;
#14128 = CARTESIAN_POINT ( 'NONE',  ( 8.409691417683177406, -21.63647391050456648, 4.520995438708348857 ) ) ;
#14129 = CARTESIAN_POINT ( 'NONE',  ( -5.215308582316793284, -23.77099543870833998, 2.825813738724734847 ) ) ;
#14130 = VERTEX_POINT ( 'NONE', #2875 ) ;
#14131 = CARTESIAN_POINT ( 'NONE',  ( 13.37500000000002132, -19.49999999999450040, 3.833333333368183382 ) ) ;
#14132 = CARTESIAN_POINT ( 'NONE',  ( -1.513434189748285696, -9.114917468222230923, 1.622643865078341463 ) ) ;
#14133 = VERTEX_POINT ( 'NONE', #10833 ) ;
#14134 = VECTOR ( 'NONE', #12854, 1000.000000000000000 ) ;
#14135 = ORIENTED_EDGE ( 'NONE', *, *, #9098, .F. ) ;
#14136 = CARTESIAN_POINT ( 'NONE',  ( 0.000000000000000000, 11.64110105645932691, 10.00000000000000000 ) ) ;
#14137 = CARTESIAN_POINT ( 'NONE',  ( -12.63819864697926754, -19.58346832754827105, 5.450273968536036406 ) ) ;
#14138 = CARTESIAN_POINT ( 'NONE',  ( -3.365018999794965548, -10.14078633184679923, 2.828722465802024910 ) ) ;
#14139 = CARTESIAN_POINT ( 'NONE',  ( -13.75871503850933841, -0.8723905552644914962, 5.888179699623941943 ) ) ;
#14140 = ADVANCED_FACE ( 'NONE', ( #17690 ), #3463, .T. ) ;
#14141 = CARTESIAN_POINT ( 'NONE',  ( 4.750698171653723989, 10.00000000000000000, 1.000000000000000000 ) ) ;
#14142 = CARTESIAN_POINT ( 'NONE',  ( 20.49999999999998224, -21.99999999999999645, 11.00000000000000178 ) ) ;
#14143 = DIRECTION ( 'NONE',  ( 0.000000000000000000, 0.000000000000000000, -1.000000000000000000 ) ) ;
#14144 = CARTESIAN_POINT ( 'NONE',  ( -10.43924542913431175, 16.00000000000000000, 1.000000000000000000 ) ) ;
#14145 = CARTESIAN_POINT ( 'NONE',  ( 12.92761177809936513, -5.718105205959081339, 6.548537912490751900 ) ) ;
#14146 = CARTESIAN_POINT ( 'NONE',  ( -11.59719141768317741, -23.08622137881040359, 5.979004561291654696 ) ) ;
#14147 = CARTESIAN_POINT ( 'NONE',  ( -1.862510824048270619, -9.990417728039201251, 2.404874838918925395 ) ) ;
#14148 = ORIENTED_EDGE ( 'NONE', *, *, #19539, .F. ) ;
#14149 = CARTESIAN_POINT ( 'NONE',  ( -13.37561105820882013, -20.21914156045197686, 4.753815841436231260 ) ) ;
#14150 = CARTESIAN_POINT ( 'NONE',  ( 0.3749999999999968914, 4.999999999999999112, 1.000000000000000000 ) ) ;
#14151 = CARTESIAN_POINT ( 'NONE',  ( 7.190941417683177406, -23.80360840875937001, 5.231925497173365081 ) ) ;
#14152 = CARTESIAN_POINT ( 'NONE',  ( -12.80905858231679417, -22.74294823697954016, 2.828734674606448785 ) ) ;
#14153 = ORIENTED_EDGE ( 'NONE', *, *, #15005, .T. ) ;
#14154 = CARTESIAN_POINT ( 'NONE',  ( 13.87470586348985258, 4.985146106231644225, 5.033049509202228933 ) ) ;
#14155 = CARTESIAN_POINT ( 'NONE',  ( 12.62888984277510218, -20.05356293986039873, 5.111704976569332537 ) ) ;
#14156 = DIRECTION ( 'NONE',  ( 0.000000000000000000, -1.000000000000000000, 0.000000000000000000 ) ) ;
#14157 = ORIENTED_EDGE ( 'NONE', *, *, #20652, .T. ) ;
#14158 = ADVANCED_FACE ( 'NONE', ( #15622 ), #1307, .T. ) ;
#14159 = ORIENTED_EDGE ( 'NONE', *, *, #6972, .F. ) ;
#14160 = PLANE ( 'NONE',  #20467 ) ;
#14161 = CARTESIAN_POINT ( 'NONE',  ( -13.89292490618230147, -0.3192367551084450139, 0.9728728682520063620 ) ) ;
#14162 = VERTEX_POINT ( 'NONE', #8276 ) ;
#14163 = CARTESIAN_POINT ( 'NONE',  ( 30.00000000000000000, 0.000000000000000000, 1.000000000000000000 ) ) ;
#14164 = CARTESIAN_POINT ( 'NONE',  ( 2.367358971471363649, -9.400572650371021410, 2.446005822389718087 ) ) ;
#14165 = DIRECTION ( 'NONE',  ( 1.000000000000000000, 0.000000000000000000, 0.000000000000000000 ) ) ;
#14166 = CARTESIAN_POINT ( 'NONE',  ( 1.513434189748285696, -9.114917468222230923, 1.622643865078341463 ) ) ;
#14167 = CARTESIAN_POINT ( 'NONE',  ( -9.805650798910056309, 9.000000000000001776, 0.000000000000000000 ) ) ;
#14168 = LINE ( 'NONE', #17732, #17779 ) ;
#14169 = CARTESIAN_POINT ( 'NONE',  ( 8.876396343307449754, 11.64110105645932691, 0.000000000000000000 ) ) ;
#14170 = PLANE ( 'NONE',  #5041 ) ;
#14171 = CARTESIAN_POINT ( 'NONE',  ( 6.813547257480585095, 10.00000000000000000, 1.000000000000000000 ) ) ;
#14172 = CARTESIAN_POINT ( 'NONE',  ( 7.097191417683176518, -22.46490103525075810, 4.479004561291653808 ) ) ;
#14173 = CARTESIAN_POINT ( 'NONE',  ( -13.10821839766814279, 4.152529082241303904, 5.997503362667785609 ) ) ;
#14174 = CARTESIAN_POINT ( 'NONE',  ( -8.309058582316795949, -22.74294823697954016, 2.828734674606448785 ) ) ;
#14175 = CARTESIAN_POINT ( 'NONE',  ( -12.53469141768317741, -20.22900456129164581, 2.825813738724747726 ) ) ;
#14176 = ORIENTED_EDGE ( 'NONE', *, *, #4777, .F. ) ;
#14177 = CARTESIAN_POINT ( 'NONE',  ( 13.09560264576187905, 4.265433610975056133, 4.833333333333343695 ) ) ;
#14178 = CARTESIAN_POINT ( 'NONE',  ( 7.499999999999999112, -20.29006350946107418, 5.466506350946110260 ) ) ;
#14179 = ORIENTED_EDGE ( 'NONE', *, *, #15695, .T. ) ;
#14180 = CARTESIAN_POINT ( 'NONE',  ( -9.689245429134309973, 0.000000000000000000, 0.000000000000000000 ) ) ;
#14181 = ORIENTED_EDGE ( 'NONE', *, *, #15750, .F. ) ;
#14182 = CARTESIAN_POINT ( 'NONE',  ( 0.9854920305337622199, -9.864917468222230923, 2.372643865078341019 ) ) ;
#14183 = EDGE_CURVE ( 'NONE', #13635, #14476, #7129, .T. ) ;
#14184 = ORIENTED_EDGE ( 'NONE', *, *, #19382, .F. ) ;
#14185 = CARTESIAN_POINT ( 'NONE',  ( 7.847191417683176518, -21.22443879296941915, 1.770995438708345748 ) ) ;
#14186 = LINE ( 'NONE', #9696, #8304 ) ;
#14187 = AXIS2_PLACEMENT_3D ( 'NONE', #15270, #16744, #16434 ) ;
#14188 = CARTESIAN_POINT ( 'NONE',  ( -1.862510824048270619, -9.990417728039201251, 2.404874838918925395 ) ) ;
#14189 = CARTESIAN_POINT ( 'NONE',  ( -20.00000000000000000, 3.000000000000000888, 1.500000000000000000 ) ) ;
#14190 = CARTESIAN_POINT ( 'NONE',  ( -11.77780858231679773, -20.27099543870833642, 2.724438792969431589 ) ) ;
#14191 = CARTESIAN_POINT ( 'NONE',  ( 14.50000000000000000, -20.99999999999998934, 4.000000000000000000 ) ) ;
#14192 = CARTESIAN_POINT ( 'NONE',  ( 7.472191417683177406, -24.47900456129165292, 2.413778621189595963 ) ) ;
#14193 = CARTESIAN_POINT ( 'NONE',  ( -32.65117217603048516, 6.460468870412185538, 0.000000000000000000 ) ) ;
#14194 = CARTESIAN_POINT ( 'NONE',  ( -6.815941417683176518, -20.79840458871654363, 4.773278322869464851 ) ) ;
#14195 = ORIENTED_EDGE ( 'NONE', *, *, #6171, .F. ) ;
#14196 = CARTESIAN_POINT ( 'NONE',  ( 6.621558582316794173, -23.74999999999999645, 3.550687472877651629 ) ) ;
#14197 = DIRECTION ( 'NONE',  ( 1.000000000000000000, 0.000000000000000000, 0.000000000000000000 ) ) ;
#14198 = CARTESIAN_POINT ( 'NONE',  ( -12.65679946139692902, -19.39412719945235253, 6.251687395662565372 ) ) ;
#14199 = ORIENTED_EDGE ( 'NONE', *, *, #1110, .T. ) ;
#14200 = CARTESIAN_POINT ( 'NONE',  ( 7.652808582316795061, -21.22443879296942626, 5.229004561291659137 ) ) ;
#14201 = CARTESIAN_POINT ( 'NONE',  ( -13.17791111847408025, 4.999999999999999112, 0.000000000000000000 ) ) ;
#14202 = ORIENTED_EDGE ( 'NONE', *, *, #17853, .F. ) ;
#14203 = DIRECTION ( 'NONE',  ( 1.000000000000000000, 0.000000000000000000, 0.000000000000000000 ) ) ;
#14204 = EDGE_LOOP ( 'NONE', ( #9963, #18150, #16375, #18374 ) ) ;
#14205 = EDGE_CURVE ( 'NONE', #1368, #4668, #13081, .T. ) ;
#14206 = CARTESIAN_POINT ( 'NONE',  ( 0.000000000000000000, 9.000000000000001776, 1.000000000000000000 ) ) ;
#14207 = ORIENTED_EDGE ( 'NONE', *, *, #11198, .T. ) ;
#14208 = CARTESIAN_POINT ( 'NONE',  ( -5.871558582316794173, -20.24999999999999289, 3.449312527122348371 ) ) ;
#14209 = CARTESIAN_POINT ( 'NONE',  ( -0.000000000000000000, 10.00000000000000000, 0.000000000000000000 ) ) ;
#14210 = EDGE_CURVE ( 'NONE', #3840, #1310, #19677, .T. ) ;
#14211 = FACE_OUTER_BOUND ( 'NONE', #4565, .T. ) ;
#14212 = CARTESIAN_POINT ( 'NONE',  ( 2.512468814886674284, -13.43512376012158782, 2.539544162874482591 ) ) ;
#14213 = EDGE_CURVE ( 'NONE', #15652, #14026, #16620, .T. ) ;
#14214 = LINE ( 'NONE', #18944, #660 ) ;
#14215 = CARTESIAN_POINT ( 'NONE',  ( -13.84311479963346869, 4.139797381492562600, 5.195993353439945395 ) ) ;
#14216 = VECTOR ( 'NONE', #3630, 1000.000000000000000 ) ;
#14217 = CARTESIAN_POINT ( 'NONE',  ( 4.746558582316793284, -21.94931252712234482, 5.250000000000000888 ) ) ;
#14218 = CARTESIAN_POINT ( 'NONE',  ( -12.62927505847832776, -20.78410954684871825, 5.373974324164845662 ) ) ;
#14219 = CARTESIAN_POINT ( 'NONE',  ( -13.12529397354238192, 5.014845663890297622, 3.999999999999981792 ) ) ;
#14220 = CARTESIAN_POINT ( 'NONE',  ( 6.059058582316793284, -20.72672167713054137, 4.701595411283463477 ) ) ;
#14221 = CARTESIAN_POINT ( 'NONE',  ( 4.284691417683177406, -23.02099543870834353, 3.863526089495429972 ) ) ;
#14222 = CARTESIAN_POINT ( 'NONE',  ( -12.25344141768317741, -21.94931252712233061, 1.749999999999998446 ) ) ;
#14223 = ORIENTED_EDGE ( 'NONE', *, *, #3216, .F. ) ;
#14224 = CARTESIAN_POINT ( 'NONE',  ( 13.64827103573800571, -5.699812695207630675, 5.034333296717131034 ) ) ;
#14225 = DIRECTION ( 'NONE',  ( -1.000000000000000000, 0.000000000000000000, 0.000000000000000000 ) ) ;
#14226 = ORIENTED_EDGE ( 'NONE', *, *, #17638, .F. ) ;
#14227 = ADVANCED_FACE ( 'NONE', ( #3563 ), #9943, .T. ) ;
#14228 = ORIENTED_EDGE ( 'NONE', *, *, #19502, .T. ) ;
#14229 = CARTESIAN_POINT ( 'NONE',  ( 0.000000000000000000, 16.00000000000000000, 1.000000000000000000 ) ) ;
#14230 = LINE ( 'NONE', #11115, #5933 ) ;
#14231 = CARTESIAN_POINT ( 'NONE',  ( -3.951988298270009636, -13.15210598010094323, 2.852089508627633219 ) ) ;
#14232 = CARTESIAN_POINT ( 'NONE',  ( 1.407845757905374695, -9.114917468222230923, 2.372643865078341019 ) ) ;
#14233 = CYLINDRICAL_SURFACE ( 'NONE', #7394, 0.3749999999999997224 ) ;
#14234 = CARTESIAN_POINT ( 'NONE',  ( 24.62918902992234038, 16.00000000000000000, 1.000000000000000000 ) ) ;
#14235 = CARTESIAN_POINT ( 'NONE',  ( 10.84030858231679240, -22.67418626127525982, 5.270995438708342640 ) ) ;
#14236 = LINE ( 'NONE', #16031, #9401 ) ;
#14237 = CARTESIAN_POINT ( 'NONE',  ( 12.96597876160390683, -3.780572539034193102, 6.590204579154564257 ) ) ;
#14238 = ADVANCED_FACE ( 'NONE', ( #15061 ), #3873, .F. ) ;
#14239 = CARTESIAN_POINT ( 'NONE',  ( -10.56594141768317741, -23.73192549717336064, 1.696391591240623331 ) ) ;
#14240 = CARTESIAN_POINT ( 'NONE',  ( -0.9854920305337622199, -9.864917468222230923, 1.622643865078341907 ) ) ;
#14241 = ORIENTED_EDGE ( 'NONE', *, *, #9614, .F. ) ;
#14242 = CARTESIAN_POINT ( 'NONE',  ( -13.84501469867711698, 4.235742283194553259, 2.999999999999999556 ) ) ;
#14243 = DIRECTION ( 'NONE',  ( 1.000000000000000000, 0.000000000000000000, 0.000000000000000000 ) ) ;
#14244 = CARTESIAN_POINT ( 'NONE',  ( 12.44094141768317741, -20.72672167713052715, 2.298404588716546293 ) ) ;
#14245 = CARTESIAN_POINT ( 'NONE',  ( -10.84030858231679595, -22.36352608949544418, 4.520995438708343528 ) ) ;
#14246 = EDGE_LOOP ( 'NONE', ( #6582, #3513, #15026, #287 ) ) ;
#14247 = CARTESIAN_POINT ( 'NONE',  ( 13.87470602645761986, 4.985154336109792972, 4.666666666666619889 ) ) ;
#14248 = CARTESIAN_POINT ( 'NONE',  ( 12.64195242771744709, -19.39390240027112000, 5.496549442168085164 ) ) ;
#14249 = PLANE ( 'NONE',  #4656 ) ;
#14250 = ORIENTED_EDGE ( 'NONE', *, *, #14858, .T. ) ;
#14251 = EDGE_CURVE ( 'NONE', #6572, #3927, #11918, .T. ) ;
#14252 = VERTEX_POINT ( 'NONE', #13182 ) ;
#14253 = ADVANCED_FACE ( 'NONE', ( #5341 ), #3977, .T. ) ;
#14254 = CARTESIAN_POINT ( 'NONE',  ( 14.00000000000000000, 7.867487981852999499E-15, 2.000000000000000000 ) ) ;
#14255 = CARTESIAN_POINT ( 'NONE',  ( -30.00000000000000000, 0.000000000000000000, 1.000000000000000000 ) ) ;
#14256 = VECTOR ( 'NONE', #204, 1000.000000000000000 ) ;
#14257 = ORIENTED_EDGE ( 'NONE', *, *, #5268, .F. ) ;
#14258 = CARTESIAN_POINT ( 'NONE',  ( -4.315753587183824180, -21.65797192216093947, 4.831781436261117335 ) ) ;
#14259 = CARTESIAN_POINT ( 'NONE',  ( 2.731427961995660958, -10.89409100229510052, 2.829571171190552015 ) ) ;
#14260 = CARTESIAN_POINT ( 'NONE',  ( 0.000000000000000000, 10.00000000000000000, 1.000000000000000000 ) ) ;
#14261 = CARTESIAN_POINT ( 'NONE',  ( 1.548630333695928618, -8.364917468222230923, 1.622643865078341907 ) ) ;
#14262 = DIRECTION ( 'NONE',  ( 0.000000000000000000, 1.000000000000000000, -0.000000000000000000 ) ) ;
#14263 = VECTOR ( 'NONE', #19043, 1000.000000000000000 ) ;
#14264 = LINE ( 'NONE', #17514, #13096 ) ;
#14265 = EDGE_CURVE ( 'NONE', #12176, #6649, #10361, .T. ) ;
#14266 = DIRECTION ( 'NONE',  ( 0.000000000000000000, 0.2487476929738665354, 0.9685683172808094987 ) ) ;
#14267 = LINE ( 'NONE', #7903, #4303 ) ;
#14268 = CARTESIAN_POINT ( 'NONE',  ( -11.96530858231679595, -20.22900456129164937, 4.174186261275266929 ) ) ;
#14269 = CARTESIAN_POINT ( 'NONE',  ( -22.06633994409548194, 0.000000000000000000, 1.000000000000000000 ) ) ;
#14270 = CARTESIAN_POINT ( 'NONE',  ( 6.815941417683177406, -21.32873467460645145, 4.242948236979555254 ) ) ;
#14271 = CARTESIAN_POINT ( 'NONE',  ( -13.02818618459764188, 0.1109023222084986743, 5.923858176248589125 ) ) ;
#14272 = CARTESIAN_POINT ( 'NONE',  ( -12.62155858231679417, -23.74999999999999645, 3.550687472877651629 ) ) ;
#14273 = CARTESIAN_POINT ( 'NONE',  ( -11.87844141768317563, -23.74999999999999645, 3.449312527122335492 ) ) ;
#14274 = ORIENTED_EDGE ( 'NONE', *, *, #17834, .F. ) ;
#14275 = CARTESIAN_POINT ( 'NONE',  ( 13.37500000000002132, -19.50000000000273559, 4.083333333315724012 ) ) ;
#14276 = CARTESIAN_POINT ( 'NONE',  ( 14.31494360078803041, 11.64110105645932691, 0.000000000000000000 ) ) ;
#14277 = ORIENTED_EDGE ( 'NONE', *, *, #14365, .F. ) ;
#14278 = VECTOR ( 'NONE', #13880, 1000.000000000000000 ) ;
#14279 = DIRECTION ( 'NONE',  ( -0.000000000000000000, -0.000000000000000000, -1.000000000000000000 ) ) ;
#14280 = ORIENTED_EDGE ( 'NONE', *, *, #4442, .T. ) ;
#14281 = FACE_OUTER_BOUND ( 'NONE', #7327, .T. ) ;
#14282 = VERTEX_POINT ( 'NONE', #5233 ) ;
#14283 = CARTESIAN_POINT ( 'NONE',  ( 11.22219141768317741, -20.27099543870833998, 4.275561207030583510 ) ) ;
#14284 = CARTESIAN_POINT ( 'NONE',  ( 0.000000000000000000, 9.000000000000000000, 1.000000000000000000 ) ) ;
#14285 = CARTESIAN_POINT ( 'NONE',  ( -1.716273078461125090, -9.866787073280026021, 2.373124017006284170 ) ) ;
#14286 = CARTESIAN_POINT ( 'NONE',  ( 0.000000000000000000, 10.00000000000000000, 1.000000000000000000 ) ) ;
#14287 = CARTESIAN_POINT ( 'NONE',  ( -13.27780858231679595, -20.27099543870833642, 2.724438792969431589 ) ) ;
#14288 = EDGE_CURVE ( 'NONE', #16270, #9560, #16735, .T. ) ;
#14289 = PRESENTATION_LAYER_ASSIGNMENT (  '', '', ( #8290 ) ) ;
#14290 = SURFACE_STYLE_USAGE ( .BOTH. , #17445 ) ;
#14291 = CARTESIAN_POINT ( 'NONE',  ( 8.690941417683177406, -23.80360840875937001, 5.231925497173365081 ) ) ;
#14292 = CARTESIAN_POINT ( 'NONE',  ( -13.12529397354238192, 5.014845663890295846, 4.166666666666765551 ) ) ;
#14293 = CARTESIAN_POINT ( 'NONE',  ( -10.47219141768317563, -23.72900456129165292, 2.724438792969417822 ) ) ;
#14294 = ORIENTED_EDGE ( 'NONE', *, *, #1366, .T. ) ;
#14295 = CARTESIAN_POINT ( 'NONE',  ( 9.246558582316794173, -21.94931252712234482, 5.250000000000000888 ) ) ;
#14296 = DIRECTION ( 'NONE',  ( -1.000000000000000000, -0.000000000000000000, -0.000000000000000000 ) ) ;
#14297 = CARTESIAN_POINT ( 'NONE',  ( -12.67822638532683577, -18.31206754099172684, 6.277704579156187847 ) ) ;
#14298 = ORIENTED_EDGE ( 'NONE', *, *, #16083, .F. ) ;
#14299 = CARTESIAN_POINT ( 'NONE',  ( 8.402808582316794173, -22.77556120703056308, 1.770995438708339975 ) ) ;
#14300 = CARTESIAN_POINT ( 'NONE',  ( 13.12529397354238192, 5.014845663890297622, 3.999999999999981792 ) ) ;
#14301 = ORIENTED_EDGE ( 'NONE', *, *, #16581, .F. ) ;
#14302 = ADVANCED_FACE ( 'NONE', ( #531 ), #14647, .T. ) ;
#14303 = VECTOR ( 'NONE', #13010, 1000.000000000000000 ) ;
#14304 = LINE ( 'NONE', #2926, #14940 ) ;
#14305 = ORIENTED_EDGE ( 'NONE', *, *, #15540, .T. ) ;
#14306 = AXIS2_PLACEMENT_3D ( 'NONE', #16062, #1523, #17737 ) ;
#14307 = LINE ( 'NONE', #7844, #14471 ) ;
#14308 = VECTOR ( 'NONE', #2807, 1000.000000000000000 ) ;
#14309 = EDGE_LOOP ( 'NONE', ( #2874, #388, #2558, #3951 ) ) ;
#14310 = CIRCLE ( 'NONE', #9647, 1.499999999999996225 ) ;
#14311 = CARTESIAN_POINT ( 'NONE',  ( -12.05905858231679595, -20.19639159124062999, 5.231925497173373074 ) ) ;
#14312 = CARTESIAN_POINT ( 'NONE',  ( 12.64323021897839006, -19.32937394158751943, 5.504219675487169283 ) ) ;
#14313 = CARTESIAN_POINT ( 'NONE',  ( 4.000698171653723101, 0.000000000000000000, 1.000000000000000000 ) ) ;
#14314 = CARTESIAN_POINT ( 'NONE',  ( 2.442511739767545098, -14.09457879449248807, 3.458905389639174821 ) ) ;
#14315 = VECTOR ( 'NONE', #3218, 1000.000000000000000 ) ;
#14316 = CARTESIAN_POINT ( 'NONE',  ( 11.00000000000000000, -18.49999999999999645, 6.500000000000000888 ) ) ;
#14317 = CARTESIAN_POINT ( 'NONE',  ( -13.38569699238614952, -18.95980188449660986, 4.749177046715717054 ) ) ;
#14318 = AXIS2_PLACEMENT_3D ( 'NONE', #8421, #3807, #6941 ) ;
#14319 = CARTESIAN_POINT ( 'NONE',  ( 7.371558582316794173, -20.24999999999999289, 3.449312527122348371 ) ) ;
#14320 = CARTESIAN_POINT ( 'NONE',  ( -12.66144083004408571, -19.15973808277258073, 6.259475412489329038 ) ) ;
#14321 = EDGE_CURVE ( 'NONE', #7216, #20520, #6146, .T. ) ;
#14322 = VECTOR ( 'NONE', #16614, 1000.000000000000000 ) ;
#14323 = CARTESIAN_POINT ( 'NONE',  ( -5.433390479346035029, 0.000000000000000000, 1.000000000000000000 ) ) ;
#14324 = CARTESIAN_POINT ( 'NONE',  ( -5.309058582316795949, -23.80360840875935935, 1.768074502826626260 ) ) ;
#14325 = CARTESIAN_POINT ( 'NONE',  ( 7.184058582316794173, -20.79840458871652942, 2.226721677130544030 ) ) ;
#14326 = CARTESIAN_POINT ( 'NONE',  ( 8.034691417683175629, -20.97900456129164581, 3.136473910504570917 ) ) ;
#14327 = CARTESIAN_POINT ( 'NONE',  ( -11.50344141768317563, -22.05068747287765873, 5.250000000000000888 ) ) ;
#14328 = ORIENTED_EDGE ( 'NONE', *, *, #18899, .F. ) ;
#14329 = EDGE_CURVE ( 'NONE', #1636, #2453, #2199, .T. ) ;
#14330 = CARTESIAN_POINT ( 'NONE',  ( 13.37515323800563039, -20.24226148071262799, 4.627790572011877934 ) ) ;
#14331 = EDGE_CURVE ( 'NONE', #16862, #5029, #17998, .T. ) ;
#14332 = DIRECTION ( 'NONE',  ( 0.000000000000000000, -1.000000000000000000, 0.000000000000000000 ) ) ;
#14333 = VERTEX_POINT ( 'NONE', #2102 ) ;
#14334 = ORIENTED_EDGE ( 'NONE', *, *, #2999, .F. ) ;
#14335 = DIRECTION ( 'NONE',  ( -1.734723475976807094E-15, -1.000000000000000000, 0.000000000000000000 ) ) ;
#14336 = VECTOR ( 'NONE', #15432, 1000.000000000000000 ) ;
#14337 = DIRECTION ( 'NONE',  ( 1.000000000000000000, 0.000000000000000000, -0.000000000000000000 ) ) ;
#14338 = CARTESIAN_POINT ( 'NONE',  ( 13.37327929115833669, -20.24999999707183207, 3.449077790995325632 ) ) ;
#14339 = AXIS2_PLACEMENT_3D ( 'NONE', #3695, #13003, #13106 ) ;
#14340 = AXIS2_PLACEMENT_3D ( 'NONE', #6033, #12405, #18799 ) ;
#14341 = CARTESIAN_POINT ( 'NONE',  ( -3.636036383999129207, -10.90885478516162976, 2.275977788322152584 ) ) ;
#14342 = CARTESIAN_POINT ( 'NONE',  ( -27.50000000000000355, 3.000000000000000888, 0.000000000000000000 ) ) ;
#14343 = VECTOR ( 'NONE', #15153, 1000.000000000000000 ) ;
#14344 = CARTESIAN_POINT ( 'NONE',  ( 2.708677329869237482, -9.785633270066144362, 1.794897081886200230 ) ) ;
#14345 = CARTESIAN_POINT ( 'NONE',  ( -13.06655316810189227, 2.048434989138931961, 5.965524842914772030 ) ) ;
#14346 = CARTESIAN_POINT ( 'NONE',  ( 9.809058582316794173, -23.27327832286945153, 2.298404588716537411 ) ) ;
#14347 = DIRECTION ( 'NONE',  ( 1.000000000000000000, 0.000000000000000000, 0.000000000000000000 ) ) ;
#14348 = CARTESIAN_POINT ( 'NONE',  ( 13.07148796623841847, 1.547642295024179493, 6.704787912489258872 ) ) ;
#14349 = EDGE_CURVE ( 'NONE', #10513, #13481, #7020, .T. ) ;
#14350 = CARTESIAN_POINT ( 'NONE',  ( -2.031432063436913182, -10.08997855658269671, 1.680444048616273722 ) ) ;
#14351 = EDGE_LOOP ( 'NONE', ( #1916, #10603, #9413, #6349 ) ) ;
#14352 = CARTESIAN_POINT ( 'NONE',  ( -13.85723511636018301, 4.102873376188801657, 5.986996695041598926 ) ) ;
#14353 = CARTESIAN_POINT ( 'NONE',  ( 24.62918902992234038, 0.000000000000000000, 1.000000000000000000 ) ) ;
#14354 = CARTESIAN_POINT ( 'NONE',  ( 9.159691417683175629, -22.98484643305507191, 0.9790045612916508100 ) ) ;
#14355 = CARTESIAN_POINT ( 'NONE',  ( -11.30905858231679595, -22.74294823697954016, 2.828734674606448785 ) ) ;
#14356 = MECHANICAL_DESIGN_GEOMETRIC_PRESENTATION_REPRESENTATION (  '', ( #2005 ), #16704 ) ;
#14357 = ORIENTED_EDGE ( 'NONE', *, *, #1560, .F. ) ;
#14358 = CARTESIAN_POINT ( 'NONE',  ( 13.90439706815434739, 5.734551941788608609, 5.045486763335835789 ) ) ;
#14359 = CARTESIAN_POINT ( 'NONE',  ( 12.74043380832193684, -14.42059267975384529, 5.611358176248560703 ) ) ;
#14360 = FACE_OUTER_BOUND ( 'NONE', #13842, .T. ) ;
#14361 = VERTEX_POINT ( 'NONE', #11819 ) ;
#14362 = AXIS2_PLACEMENT_3D ( 'NONE', #5039, #14337, #19279 ) ;
#14363 = ORIENTED_EDGE ( 'NONE', *, *, #4048, .T. ) ;
#14364 = FACE_OUTER_BOUND ( 'NONE', #12896, .T. ) ;
#14365 = EDGE_CURVE ( 'NONE', #11436, #7048, #10251, .T. ) ;
#14366 = CARTESIAN_POINT ( 'NONE',  ( 0.000000000000000000, 10.00000000000000000, 1.000000000000000000 ) ) ;
#14367 = DIRECTION ( 'NONE',  ( -1.000000000000000000, 0.000000000000000000, 0.000000000000000000 ) ) ;
#14368 = CARTESIAN_POINT ( 'NONE',  ( -13.12529397354238192, 5.014845663890297622, 3.999999999999981792 ) ) ;
#14369 = FACE_OUTER_BOUND ( 'NONE', #18523, .T. ) ;
#14370 = CARTESIAN_POINT ( 'NONE',  ( 2.327620134574780231, -13.27885108724501251, 3.249410218619480872 ) ) ;
#14371 = DIRECTION ( 'NONE',  ( 0.000000000000000000, -1.000000000000000000, 0.000000000000000000 ) ) ;
#14372 = CARTESIAN_POINT ( 'NONE',  ( 20.00000000000000000, 0.000000000000000000, 1.000000000000000000 ) ) ;
#14373 = AXIS2_PLACEMENT_3D ( 'NONE', #578, #5184, #6859 ) ;
#14374 = VECTOR ( 'NONE', #12909, 1000.000000000000000 ) ;
#14375 = EDGE_CURVE ( 'NONE', #10392, #10835, #12133, .T. ) ;
#14376 = DIRECTION ( 'NONE',  ( 0.000000000000000000, 0.000000000000000000, 1.000000000000000000 ) ) ;
#14377 = CARTESIAN_POINT ( 'NONE',  ( -14.56494360078803396, 0.000000000000000000, 1.000000000000000000 ) ) ;
#14378 = CARTESIAN_POINT ( 'NONE',  ( -11.49655858231679417, -22.05068747287764452, 1.749999999999998446 ) ) ;
#14379 = EDGE_CURVE ( 'NONE', #2607, #4438, #18625, .T. ) ;
#14380 = LINE ( 'NONE', #14171, #20387 ) ;
#14381 = CARTESIAN_POINT ( 'NONE',  ( 11.96530858231679773, -20.97900456129165647, 3.863526089495444626 ) ) ;
#14382 = CARTESIAN_POINT ( 'NONE',  ( -12.62746768552656285, -19.37538188090202596, 4.723115281690125400 ) ) ;
#14383 = CARTESIAN_POINT ( 'NONE',  ( -6.340308582316796837, -22.36352608949544418, 4.520995438708343528 ) ) ;
#14384 = CARTESIAN_POINT ( 'NONE',  ( -6.534691417683177406, -19.47900456129164581, 2.515153566944927199 ) ) ;
#14385 = VERTEX_POINT ( 'NONE', #7329 ) ;
#14386 = CARTESIAN_POINT ( 'NONE',  ( 13.08439876642066935, 3.699637704240349656, 5.251001356674258602 ) ) ;
#14387 = LINE ( 'NONE', #14080, #306 ) ;
#14388 = ORIENTED_EDGE ( 'NONE', *, *, #1872, .T. ) ;
#14389 = ORIENTED_EDGE ( 'NONE', *, *, #3250, .T. ) ;
#14390 = CARTESIAN_POINT ( 'NONE',  ( 0.000000000000000000, 0.000000000000000000, 4.000000000000000000 ) ) ;
#14391 = CARTESIAN_POINT ( 'NONE',  ( 13.86616162069444691, 3.803661845068127878, 6.738770894197415373 ) ) ;
#14392 = VERTEX_POINT ( 'NONE', #1055 ) ;
#14393 = LINE ( 'NONE', #2356, #12101 ) ;
#14394 = EDGE_CURVE ( 'NONE', #8920, #682, #10883, .T. ) ;
#14395 = VECTOR ( 'NONE', #12675, 999.9999999999998863 ) ;
#14396 = VECTOR ( 'NONE', #12242, 1000.000000000000000 ) ;
#14397 = ORIENTED_EDGE ( 'NONE', *, *, #7601, .F. ) ;
#14398 = CARTESIAN_POINT ( 'NONE',  ( 10.37844141768317741, -23.74999999999999645, 3.449312527122335492 ) ) ;
#14399 = DIRECTION ( 'NONE',  ( 0.000000000000000000, 0.000000000000000000, 1.000000000000000000 ) ) ;
#14400 = CARTESIAN_POINT ( 'NONE',  ( -2.602174906157317835, -9.976397331638239052, 2.593889103792902606 ) ) ;
#14401 = CARTESIAN_POINT ( 'NONE',  ( 2.731427961995660958, -10.89409100229510052, 2.829571171190552015 ) ) ;
#14402 = CARTESIAN_POINT ( 'NONE',  ( -11.02780858231679595, -23.72900456129165292, 4.275561207030568411 ) ) ;
#14403 = CARTESIAN_POINT ( 'NONE',  ( 6.815941417683177406, -20.26807450282663225, 5.303608408759377113 ) ) ;
#14404 = FACE_BOUND ( 'NONE', #2692, .T. ) ;
#14405 = CARTESIAN_POINT ( 'NONE',  ( -5.315941417683176518, -20.79840458871654363, 4.773278322869464851 ) ) ;
#14406 = AXIS2_PLACEMENT_3D ( 'NONE', #2649, #20334, #7471 ) ;
#14407 = ORIENTED_EDGE ( 'NONE', *, *, #18571, .F. ) ;
#14408 = CARTESIAN_POINT ( 'NONE',  ( 7.652808582316795061, -21.22443879296942626, 5.229004561291659137 ) ) ;
#14409 = CYLINDRICAL_SURFACE ( 'NONE', #1727, 0.4999999999999987232 ) ;
#14410 = CARTESIAN_POINT ( 'NONE',  ( -12.64183575740756993, -20.14979425091403087, 6.022201559249563907 ) ) ;
#14411 = ORIENTED_EDGE ( 'NONE', *, *, #14801, .T. ) ;
#14412 = CARTESIAN_POINT ( 'NONE',  ( 5.121558582316794173, -23.74999999999999645, 3.550687472877651629 ) ) ;
#14413 = DIRECTION ( 'NONE',  ( 0.000000000000000000, 0.000000000000000000, 1.000000000000000000 ) ) ;
#14414 = VERTEX_POINT ( 'NONE', #4285 ) ;
#14415 = LINE ( 'NONE', #9304, #584 ) ;
#14416 =( NAMED_UNIT ( * ) SI_UNIT ( $, .STERADIAN. ) SOLID_ANGLE_UNIT ( ) );
#14417 = EDGE_LOOP ( 'NONE', ( #5304, #12825, #12255, #13234 ) ) ;
#14418 = ADVANCED_FACE ( 'NONE', ( #2408 ), #12025, .T. ) ;
#14419 = LINE ( 'NONE', #8055, #18153 ) ;
#14420 = ORIENTED_EDGE ( 'NONE', *, *, #16083, .T. ) ;
#14421 = CARTESIAN_POINT ( 'NONE',  ( -12.99655858231679595, -22.05068747287764452, 0.9999999999999978906 ) ) ;
#14422 = VECTOR ( 'NONE', #14296, 1000.000000000000000 ) ;
#14423 = PLANE ( 'NONE',  #9927 ) ;
#14424 = DIRECTION ( 'NONE',  ( -0.000000000000000000, -0.000000000000000000, -1.000000000000000000 ) ) ;
#14425 = CARTESIAN_POINT ( 'NONE',  ( 2.742252025265078608, -15.06657917462210605, 2.958534504914692942 ) ) ;
#14426 = CARTESIAN_POINT ( 'NONE',  ( 13.15498566372047762, 5.764276017890828108, 4.942557026581394730 ) ) ;
#14427 = PRODUCT_RELATED_PRODUCT_CATEGORY ( 'part', '', ( #2828 ) ) ;
#14428 = CARTESIAN_POINT ( 'NONE',  ( -20.00000000000000000, -6.000000000000000000, 1.000000000000000000 ) ) ;
#14429 = CARTESIAN_POINT ( 'NONE',  ( -13.84501469867711698, 4.235742283194553259, 3.666666666666500873 ) ) ;
#14430 = CARTESIAN_POINT ( 'NONE',  ( 8.496558582316794173, -22.05068747287764452, 1.749999999999998446 ) ) ;
#14431 = VECTOR ( 'NONE', #20350, 1000.000000000000000 ) ;
#14432 = CARTESIAN_POINT ( 'NONE',  ( -12.63178515739782348, -20.65734955141111584, 5.567013446834313761 ) ) ;
#14433 = CARTESIAN_POINT ( 'NONE',  ( 0.000000000000000000, 4.999999999999999112, 1.000000000000000000 ) ) ;
#14434 = CARTESIAN_POINT ( 'NONE',  ( -10.93405858231679595, -23.73192549717337130, 5.303608408759367343 ) ) ;
#14435 = CARTESIAN_POINT ( 'NONE',  ( 7.559058582316794173, -20.72672167713054137, 4.701595411283463477 ) ) ;
#14436 = CIRCLE ( 'NONE', #10764, 10.00000000000000000 ) ;
#14437 = CARTESIAN_POINT ( 'NONE',  ( 13.27780858231679417, -21.02099543870833998, 3.035098964749253003 ) ) ;
#14438 = CARTESIAN_POINT ( 'NONE',  ( -5.972191417683177406, -23.72900456129164937, 2.724438792969417378 ) ) ;
#14439 = ORIENTED_EDGE ( 'NONE', *, *, #2109, .T. ) ;
#14440 = ORIENTED_EDGE ( 'NONE', *, *, #7773, .F. ) ;
#14441 = CARTESIAN_POINT ( 'NONE',  ( 13.37524505148396514, -20.23762490005974968, 4.659512268729234741 ) ) ;
#14442 = DIRECTION ( 'NONE',  ( 0.000000000000000000, -0.000000000000000000, 1.000000000000000000 ) ) ;
#14443 = DIRECTION ( 'NONE',  ( -1.000000000000000000, -0.000000000000000000, -0.000000000000000000 ) ) ;
#14444 = ORIENTED_EDGE ( 'NONE', *, *, #11899, .F. ) ;
#14445 = ORIENTED_EDGE ( 'NONE', *, *, #13431, .T. ) ;
#14446 = DIRECTION ( 'NONE',  ( 0.000000000000000000, 1.000000000000000000, -0.000000000000000000 ) ) ;
#14447 = DIRECTION ( 'NONE',  ( -0.000000000000000000, -0.000000000000000000, -1.000000000000000000 ) ) ;
#14448 = PLANE ( 'NONE',  #17614 ) ;
#14449 = CARTESIAN_POINT ( 'NONE',  ( -2.171407406650392780, -8.432416083433171394, 2.389978857884845986 ) ) ;
#14450 = LINE ( 'NONE', #4934, #10696 ) ;
#14451 = VECTOR ( 'NONE', #13721, 1000.000000000000000 ) ;
#14452 = EDGE_CURVE ( 'NONE', #6116, #17844, #2723, .T. ) ;
#14453 = CARTESIAN_POINT ( 'NONE',  ( 11.00000000000000000, -25.49999999999999645, 4.000000000000000000 ) ) ;
#14454 = CARTESIAN_POINT ( 'NONE',  ( -13.11740841389447709, 4.616624901677048420, 5.813473370769506765 ) ) ;
#14455 = CARTESIAN_POINT ( 'NONE',  ( 12.62155858231679417, -23.74999999999999645, 3.550687472877651629 ) ) ;
#14456 = EDGE_CURVE ( 'NONE', #19021, #14162, #8799, .T. ) ;
#14457 = CARTESIAN_POINT ( 'NONE',  ( 13.50000000000000178, 7.806255641895631925E-15, 2.000000000000000000 ) ) ;
#14458 = CARTESIAN_POINT ( 'NONE',  ( 13.15498530132288479, 5.764257716805535559, 4.166666666666765551 ) ) ;
#14459 = CARTESIAN_POINT ( 'NONE',  ( -1.709849555000590104, -9.864920124259167977, 1.622644547201689713 ) ) ;
#14460 = VERTEX_POINT ( 'NONE', #9104 ) ;
#14461 = CARTESIAN_POINT ( 'NONE',  ( -13.85223456079946303, 3.850345320370711644, 5.989742199623227847 ) ) ;
#14462 = CARTESIAN_POINT ( 'NONE',  ( -3.499999999999998668, -19.50000000000000000, 1.000000000000000000 ) ) ;
#14463 = CARTESIAN_POINT ( 'NONE',  ( 9.065941417683177406, -23.73192549717336064, 1.696391591240623331 ) ) ;
#14464 = AXIS2_PLACEMENT_3D ( 'NONE', #9826, #16211, #14627 ) ;
#14465 = CARTESIAN_POINT ( 'NONE',  ( -9.152808582316795949, -21.53509896474924901, 4.479004561291659137 ) ) ;
#14466 = ORIENTED_EDGE ( 'NONE', *, *, #417, .T. ) ;
#14467 = CARTESIAN_POINT ( 'NONE',  ( 12.62543384439201510, -20.97809085820452424, 4.782403934559678937 ) ) ;
#14468 = CARTESIAN_POINT ( 'NONE',  ( 13.10252221513633941, 3.864871864382954048, 6.004587342915129966 ) ) ;
#14469 = DIRECTION ( 'NONE',  ( 0.000000000000000000, 0.000000000000000000, 1.000000000000000000 ) ) ;
#14470 = ORIENTED_EDGE ( 'NONE', *, *, #14265, .F. ) ;
#14471 = VECTOR ( 'NONE', #10985, 1000.000000000000000 ) ;
#14472 = ORIENTED_EDGE ( 'NONE', *, *, #1492, .T. ) ;
#14473 = CARTESIAN_POINT ( 'NONE',  ( -20.75349085826862350, 0.000000000000000000, 0.000000000000000000 ) ) ;
#14474 = EDGE_CURVE ( 'NONE', #2576, #8456, #5218, .T. ) ;
#14475 = CARTESIAN_POINT ( 'NONE',  ( 22.56633994409548194, 11.64110105645932691, 10.00000000000000000 ) ) ;
#14476 = VERTEX_POINT ( 'NONE', #1158 ) ;
#14477 = EDGE_CURVE ( 'NONE', #7631, #16888, #14006, .T. ) ;
#14478 = CARTESIAN_POINT ( 'NONE',  ( -5.999999999999999112, -2.500000000000047518, 8.999999999999998224 ) ) ;
#14479 = CARTESIAN_POINT ( 'NONE',  ( 1.665360951492234287, -9.864914341757378580, 1.622643062139706993 ) ) ;
#14480 = LINE ( 'NONE', #17513, #15531 ) ;
#14481 = EDGE_CURVE ( 'NONE', #1363, #15395, #4498, .T. ) ;
#14482 = CARTESIAN_POINT ( 'NONE',  ( 0.000000000000000000, 4.999999999999999112, 1.000000000000000000 ) ) ;
#14483 = DIRECTION ( 'NONE',  ( -1.000000000000000000, 0.000000000000000000, 0.000000000000000000 ) ) ;
#14484 = FACE_OUTER_BOUND ( 'NONE', #13047, .T. ) ;
#14485 = LINE ( 'NONE', #9676, #14374 ) ;
#14486 = CARTESIAN_POINT ( 'NONE',  ( -2.731427961995660958, -10.89409100229510052, 2.829571171190552015 ) ) ;
#14487 = CARTESIAN_POINT ( 'NONE',  ( 8.027808582316795949, -22.97900456129165647, 3.964901035250747885 ) ) ;
#14488 = CARTESIAN_POINT ( 'NONE',  ( -13.09206359972826661, 4.086711786274932479, 5.245812454509717782 ) ) ;
#14489 = CARTESIAN_POINT ( 'NONE',  ( -6.621558582316796837, -22.99999999999999645, 3.550687472877652073 ) ) ;
#14490 = CARTESIAN_POINT ( 'NONE',  ( -7.003441417683177406, -22.05068747287766229, 6.000000000000001776 ) ) ;
#14491 = EDGE_LOOP ( 'NONE', ( #5286, #14148 ) ) ;
#14492 = CARTESIAN_POINT ( 'NONE',  ( 13.84311479963346869, 4.139797381492562600, 5.195993353439945395 ) ) ;
#14493 = CARTESIAN_POINT ( 'NONE',  ( 18.44064177244175440, 10.00000000000000000, 1.000000000000000000 ) ) ;
#14494 = ORIENTED_EDGE ( 'NONE', *, *, #16817, .F. ) ;
#14495 = ORIENTED_EDGE ( 'NONE', *, *, #1584, .T. ) ;
#14496 = DIRECTION ( 'NONE',  ( 5.204170427930446527E-15, -1.000000000000000000, 0.000000000000000000 ) ) ;
#14497 = ORIENTED_EDGE ( 'NONE', *, *, #5212, .T. ) ;
#14498 = CARTESIAN_POINT ( 'NONE',  ( 15.36404127825609400, 0.000000000000000000, 1.000000000000000000 ) ) ;
#14499 = ADVANCED_FACE ( 'NONE', ( #15167 ), #20099, .T. ) ;
#14500 = ORIENTED_EDGE ( 'NONE', *, *, #1338, .T. ) ;
#14501 = DIRECTION ( 'NONE',  ( 0.1351665943404306014, 0.9596796555888912339, -0.2464649070825229438 ) ) ;
#14502 = DIRECTION ( 'NONE',  ( 1.000000000000000000, 0.000000000000000000, 0.000000000000000000 ) ) ;
#14503 = CARTESIAN_POINT ( 'NONE',  ( -0.2815691515810352930, -9.114917468222230923, 2.372643865078523984 ) ) ;
#14504 = CARTESIAN_POINT ( 'NONE',  ( 2.583953725994688533, -9.847075946378776479, 2.560676788604062004 ) ) ;
#14505 = CARTESIAN_POINT ( 'NONE',  ( -13.18405858231679417, -20.79840458871652942, 2.226721677130544030 ) ) ;
#14506 = CARTESIAN_POINT ( 'NONE',  ( -15.49999999999998046, -26.49999999999999645, 4.000000000000000000 ) ) ;
#14507 = EDGE_CURVE ( 'NONE', #12054, #11489, #18525, .T. ) ;
#14508 = CARTESIAN_POINT ( 'NONE',  ( 10.37844141768317741, -23.74999999999999645, 3.449312527122335492 ) ) ;
#14509 = CARTESIAN_POINT ( 'NONE',  ( 0.000000000000000000, 0.000000000000000000, 2.000000000000000000 ) ) ;
#14510 = EDGE_CURVE ( 'NONE', #8745, #19089, #4398, .T. ) ;
#14511 = CARTESIAN_POINT ( 'NONE',  ( -6.440941417683176518, -20.72672167713052715, 2.298404588716546293 ) ) ;
#14512 = ORIENTED_EDGE ( 'NONE', *, *, #7565, .F. ) ;
#14513 = CARTESIAN_POINT ( 'NONE',  ( 11.77780858231679595, -19.52099543870833642, 2.413778621189609286 ) ) ;
#14514 = CARTESIAN_POINT ( 'NONE',  ( 12.63819864697926754, -19.58346832754827105, 5.450273968536036406 ) ) ;
#14515 = CARTESIAN_POINT ( 'NONE',  ( -13.15498530131898214, 5.764257716805535559, 3.333333333333075466 ) ) ;
#14516 = ORIENTED_EDGE ( 'NONE', *, *, #2732, .T. ) ;
#14517 = CARTESIAN_POINT ( 'NONE',  ( -6.313547257480587760, 10.00000000000000000, 0.000000000000000000 ) ) ;
#14518 = CARTESIAN_POINT ( 'NONE',  ( 25.04469207716615031, 9.000000000000001776, 1.000000000000000000 ) ) ;
#14519 = VERTEX_POINT ( 'NONE', #20301 ) ;
#14520 = PRODUCT_DEFINITION_SHAPE ( 'NONE', 'NONE',  #15961 ) ;
#14521 = PRODUCT_CONTEXT ( 'NONE', #12272, 'mechanical' ) ;
#14522 = VERTEX_POINT ( 'NONE', #9001 ) ;
#14523 = EDGE_CURVE ( 'NONE', #1363, #12435, #7225, .T. ) ;
#14524 = DIRECTION ( 'NONE',  ( -1.000000000000000000, 0.000000000000000000, -0.000000000000000000 ) ) ;
#14525 = EDGE_CURVE ( 'NONE', #1942, #868, #4185, .T. ) ;
#14526 = VECTOR ( 'NONE', #14764, 1000.000000000000000 ) ;
#14527 = ORIENTED_EDGE ( 'NONE', *, *, #18401, .T. ) ;
#14528 = CARTESIAN_POINT ( 'NONE',  ( -7.371558582316794173, -20.24999999999999289, 3.449312527122348371 ) ) ;
#14529 = LINE ( 'NONE', #14209, #4580 ) ;
#14530 = FACE_OUTER_BOUND ( 'NONE', #9684, .T. ) ;
#14531 = CARTESIAN_POINT ( 'NONE',  ( 2.627360420079438263, -14.25085146736906339, 2.749039333894452763 ) ) ;
#14532 = CARTESIAN_POINT ( 'NONE',  ( 13.15498530132288479, 5.764257716805535559, 3.666666666666500873 ) ) ;
#14533 = DIRECTION ( 'NONE',  ( 1.000000000000000000, 0.000000000000000000, 0.000000000000000000 ) ) ;
#14534 = CARTESIAN_POINT ( 'NONE',  ( -13.84501469867711698, 4.235742283194553259, 4.916666666666649199 ) ) ;
#14535 = CARTESIAN_POINT ( 'NONE',  ( 8.871558582316795949, -19.49999999999998934, 3.449312527122348371 ) ) ;
#14536 = CARTESIAN_POINT ( 'NONE',  ( -12.62499999999998579, -20.24999999999999289, 3.666666666666653640 ) ) ;
#14537 = EDGE_CURVE ( 'NONE', #4233, #13991, #12336, .T. ) ;
#14538 = DIRECTION ( 'NONE',  ( -0.000000000000000000, 0.000000000000000000, 1.000000000000000000 ) ) ;
#14539 = CARTESIAN_POINT ( 'NONE',  ( 6.152808582316793284, -21.22443879296942626, 5.229004561291659137 ) ) ;
#14540 = VECTOR ( 'NONE', #15482, 1000.000000000000000 ) ;
#14541 = STYLED_ITEM ( 'NONE', ( #6060 ), #10862 ) ;
#14542 = CARTESIAN_POINT ( 'NONE',  ( 5.315941417683176518, -21.32873467460645145, 4.242948236979555254 ) ) ;
#14543 = CARTESIAN_POINT ( 'NONE',  ( -8.878441417683177406, -23.74999999999999645, 3.449312527122335492 ) ) ;
#14544 = ORIENTED_EDGE ( 'NONE', *, *, #4493, .T. ) ;
#14545 = EDGE_LOOP ( 'NONE', ( #20044, #3214 ) ) ;
#14546 = CARTESIAN_POINT ( 'NONE',  ( 13.37499999999998401, -20.24999999999998934, 2.439580858552613751 ) ) ;
#14547 = LINE ( 'NONE', #9252, #7101 ) ;
#14548 = ORIENTED_EDGE ( 'NONE', *, *, #15760, .F. ) ;
#14549 = ORIENTED_EDGE ( 'NONE', *, *, #11197, .F. ) ;
#14550 = DIRECTION ( 'NONE',  ( 1.000000000000000000, 0.000000000000000000, 0.000000000000000000 ) ) ;
#14551 = DIRECTION ( 'NONE',  ( 0.000000000000000000, 1.000000000000000000, 0.000000000000000000 ) ) ;
#14552 = CARTESIAN_POINT ( 'NONE',  ( -13.11740841389447709, 4.616624901677048420, 5.813473370769506765 ) ) ;
#14553 = CARTESIAN_POINT ( 'NONE',  ( -2.121089610268797276, -8.411987239090384705, 1.634732322550447758 ) ) ;
#14554 = LINE ( 'NONE', #3759, #15357 ) ;
#14555 = CARTESIAN_POINT ( 'NONE',  ( -24.87918902992234393, 11.64110105645932691, 10.00000000000000000 ) ) ;
#14556 = CARTESIAN_POINT ( 'NONE',  ( -12.69247507894198712, -16.84250851341299082, 5.559274842915185033 ) ) ;
#14557 = CARTESIAN_POINT ( 'NONE',  ( 7.090308582316795061, -21.32581373872472952, 1.729004561291657138 ) ) ;
#14558 = CARTESIAN_POINT ( 'NONE',  ( -2.061130159782011972, 4.999999999999999112, 1.000000000000000000 ) ) ;
#14559 = CARTESIAN_POINT ( 'NONE',  ( 12.62499999999998224, -20.24999999999998934, 4.291666666666698937 ) ) ;
#14560 = CARTESIAN_POINT ( 'NONE',  ( -1.711347482507859397, -9.865394108634699677, 1.622766275858107621 ) ) ;
#14561 = ORIENTED_EDGE ( 'NONE', *, *, #2577, .T. ) ;
#14562 = CARTESIAN_POINT ( 'NONE',  ( -13.41820805991576826, -18.06799297425606454, 5.518388032956592859 ) ) ;
#14563 = LINE ( 'NONE', #14668, #11064 ) ;
#14564 = EDGE_CURVE ( 'NONE', #11135, #4871, #5864, .T. ) ;
#14565 = CARTESIAN_POINT ( 'NONE',  ( 8.878441417683177406, -24.50000000000000000, 3.449312527122335048 ) ) ;
#14566 = CARTESIAN_POINT ( 'NONE',  ( -5.309058582316795949, -22.74294823697954016, 2.828734674606448785 ) ) ;
#14567 = EDGE_LOOP ( 'NONE', ( #1052, #6988, #8229, #10460 ) ) ;
#14568 = CARTESIAN_POINT ( 'NONE',  ( 13.86616162069444691, 3.803661845068127878, 6.738770894197415373 ) ) ;
#14569 = CARTESIAN_POINT ( 'NONE',  ( 12.64751377014909828, -19.11305460747000495, 5.510446717915143289 ) ) ;
#14570 = DIRECTION ( 'NONE',  ( -0.000000000000000000, -0.000000000000000000, -1.000000000000000000 ) ) ;
#14571 = ORIENTED_EDGE ( 'NONE', *, *, #12271, .T. ) ;
#14572 = VERTEX_POINT ( 'NONE', #4083 ) ;
#14573 = DIRECTION ( 'NONE',  ( -0.000000000000000000, -0.000000000000000000, -1.000000000000000000 ) ) ;
#14574 = LINE ( 'NONE', #15934, #555 ) ;
#14575 = ORIENTED_EDGE ( 'NONE', *, *, #19609, .T. ) ;
#14576 = DIRECTION ( 'NONE',  ( -1.000000000000000000, 0.000000000000000000, 0.000000000000000000 ) ) ;
#14577 = CARTESIAN_POINT ( 'NONE',  ( 0.5631383031621635116, -9.114917468222230923, 1.622643865078341463 ) ) ;
#14578 = FACE_OUTER_BOUND ( 'NONE', #19967, .T. ) ;
#14579 = DIRECTION ( 'NONE',  ( 0.000000000000000000, 0.000000000000000000, 1.000000000000000000 ) ) ;
#14580 = LINE ( 'NONE', #255, #6703 ) ;
#14581 = PLANE ( 'NONE',  #9971 ) ;
#14582 = CARTESIAN_POINT ( 'NONE',  ( -11.68405858231679417, -20.79840458871652942, 2.226721677130544030 ) ) ;
#14583 = CARTESIAN_POINT ( 'NONE',  ( -2.513306525444908512, -9.622685169956881168, 2.503048754562789746 ) ) ;
#14584 = VERTEX_POINT ( 'NONE', #18835 ) ;
#14585 = CARTESIAN_POINT ( 'NONE',  ( -12.66835678905406049, -17.31048215276408797, 4.799178440007564994 ) ) ;
#14586 = CARTESIAN_POINT ( 'NONE',  ( -12.15280858231679595, -21.22443879296942626, 5.229004561291659137 ) ) ;
#14587 = ADVANCED_FACE ( 'NONE', ( #10471 ), #16838, .F. ) ;
#14588 = CARTESIAN_POINT ( 'NONE',  ( -4.378441417683176518, -23.74999999999999645, 3.449312527122335492 ) ) ;
#14589 = VERTEX_POINT ( 'NONE', #9509 ) ;
#14590 = CARTESIAN_POINT ( 'NONE',  ( 13.38269957179998038, -19.11117162410040038, 4.745921838382382241 ) ) ;
#14591 = CARTESIAN_POINT ( 'NONE',  ( 13.49999999999998401, -25.49999999999999645, 4.000000000000000000 ) ) ;
#14592 = ORIENTED_EDGE ( 'NONE', *, *, #5687, .T. ) ;
#14593 = ORIENTED_EDGE ( 'NONE', *, *, #972, .F. ) ;
#14594 = CARTESIAN_POINT ( 'NONE',  ( 21.25349085826861995, 0.000000000000000000, 1.000000000000000000 ) ) ;
#14595 = VERTEX_POINT ( 'NONE', #15680 ) ;
#14596 = CARTESIAN_POINT ( 'NONE',  ( 0.000000000000000000, 10.00000000000000000, 1.000000000000000000 ) ) ;
#14597 = EDGE_CURVE ( 'NONE', #1770, #2917, #15984, .T. ) ;
#14598 = EDGE_CURVE ( 'NONE', #18281, #19766, #7936, .T. ) ;
#14599 = ORIENTED_EDGE ( 'NONE', *, *, #1425, .T. ) ;
#14600 = CARTESIAN_POINT ( 'NONE',  ( 11.50344141768317563, -22.05068747287765873, 5.250000000000000888 ) ) ;
#14601 = LINE ( 'NONE', #13038, #13996 ) ;
#14602 = CARTESIAN_POINT ( 'NONE',  ( -2.109407804498405703, -9.207748739546751438, 2.396484790045401603 ) ) ;
#14603 = DIRECTION ( 'NONE',  ( 1.000000000000000000, 0.000000000000000000, 0.000000000000000000 ) ) ;
#14604 = CARTESIAN_POINT ( 'NONE',  ( -9.434058582316794173, -23.20159541128345992, 4.773278322869455970 ) ) ;
#14605 = LINE ( 'NONE', #12833, #19992 ) ;
#14606 = CARTESIAN_POINT ( 'NONE',  ( 11.40969141768318096, -21.32581373872474373, 5.270995438708348857 ) ) ;
#14607 = FACE_OUTER_BOUND ( 'NONE', #4455, .T. ) ;
#14608 = CARTESIAN_POINT ( 'NONE',  ( -3.944195004867016241, -21.61378581760806838, 5.207602947182413899 ) ) ;
#14609 = EDGE_CURVE ( 'NONE', #2020, #8434, #14415, .T. ) ;
#14610 = VERTEX_POINT ( 'NONE', #17246 ) ;
#14611 = CARTESIAN_POINT ( 'NONE',  ( 8.215308582316795949, -24.52099543870834708, 2.515153566944913432 ) ) ;
#14612 = CARTESIAN_POINT ( 'NONE',  ( 12.64323021897839006, -19.32937394158751943, 5.504219675487169283 ) ) ;
#14613 = CARTESIAN_POINT ( 'NONE',  ( -13.15316049959406364, 5.672105229501871904, 5.573635960501007958 ) ) ;
#14614 = ORIENTED_EDGE ( 'NONE', *, *, #254, .T. ) ;
#14615 = CIRCLE ( 'NONE', #5605, 10.00000000000000000 ) ;
#14616 = CARTESIAN_POINT ( 'NONE',  ( -7.499999999999999112, -25.49999999999999645, 6.500000000000000888 ) ) ;
#14617 = DIRECTION ( 'NONE',  ( -0.000000000000000000, -0.000000000000000000, -1.000000000000000000 ) ) ;
#14618 = VERTEX_POINT ( 'NONE', #9412 ) ;
#14619 = SHAPE_REPRESENTATION_RELATIONSHIP ( 'NONE' , 'NONE' ,  #6045, #4794 ) ;
#14620 = VERTEX_POINT ( 'NONE', #1462 ) ;
#14621 = CARTESIAN_POINT ( 'NONE',  ( 8.126396343307449754, 16.00000000000000000, 1.000000000000000000 ) ) ;
#14622 = ORIENTED_EDGE ( 'NONE', *, *, #16412, .T. ) ;
#14623 = EDGE_CURVE ( 'NONE', #19766, #11965, #1558, .T. ) ;
#14624 = CARTESIAN_POINT ( 'NONE',  ( -12.71530858231679417, -24.52099543870834708, 2.515153566944913432 ) ) ;
#14625 = CARTESIAN_POINT ( 'NONE',  ( 13.11145189917479392, 4.315820908324673688, 5.961432613039677086 ) ) ;
#14626 = VECTOR ( 'NONE', #17646, 1000.000000000000000 ) ;
#14627 = DIRECTION ( 'NONE',  ( 1.000000000000000000, 0.000000000000000000, 0.000000000000000000 ) ) ;
#14628 = CARTESIAN_POINT ( 'NONE',  ( 12.62524871736568954, -20.23743977303344010, 4.661898514667671023 ) ) ;
#14629 = DIRECTION ( 'NONE',  ( 0.000000000000000000, 1.000000000000000000, -0.000000000000000000 ) ) ;
#14630 = CARTESIAN_POINT ( 'NONE',  ( -13.84042474920106081, 4.003949834653575124, 5.242612001278796008 ) ) ;
#14631 = CARTESIAN_POINT ( 'NONE',  ( 10.46530858231679595, -19.47900456129164937, 4.484846433055089676 ) ) ;
#14632 = CARTESIAN_POINT ( 'NONE',  ( -13.15047398821051239, 5.536436404627260721, 5.896317606305554015 ) ) ;
#14633 = CARTESIAN_POINT ( 'NONE',  ( -10.09719141768317741, -23.08622137881040359, 5.979004561291654696 ) ) ;
#14634 = EDGE_CURVE ( 'NONE', #14460, #5550, #14304, .T. ) ;
#14635 = ADVANCED_FACE ( 'NONE', ( #6169 ), #6485, .T. ) ;
#14636 = CARTESIAN_POINT ( 'NONE',  ( -11.00000000000000000, -23.83493649053891517, 4.999999999999999112 ) ) ;
#14637 = CARTESIAN_POINT ( 'NONE',  ( -0.1250000000000001110, 10.00000000000000000, 0.000000000000000000 ) ) ;
#14638 = CLOSED_SHELL ( 'NONE', ( #10610, #11791, #11973, #1464, #5075, #12246, #2582, #11265, #14635, #19191, #3734, #14897, #10806, #8415, #13655, #436, #12938, #15910, #5771, #12421, #18059, #9920 ) ) ;
#14639 = VECTOR ( 'NONE', #20186, 1000.000000000000000 ) ;
#14640 = CARTESIAN_POINT ( 'NONE',  ( 7.277808582316795061, -21.02099543870833998, 3.035098964749253003 ) ) ;
#14641 = CARTESIAN_POINT ( 'NONE',  ( -7.565941417683176518, -23.20159541128344927, 2.226721677130534705 ) ) ;
#14642 = VECTOR ( 'NONE', #5660, 1000.000000000000000 ) ;
#14643 = ORIENTED_EDGE ( 'NONE', *, *, #8340, .F. ) ;
#14644 = EDGE_CURVE ( 'NONE', #13564, #911, #15272, .T. ) ;
#14645 = ORIENTED_EDGE ( 'NONE', *, *, #12135, .T. ) ;
#14646 = CARTESIAN_POINT ( 'NONE',  ( 13.37597619100657198, -20.20070235416671167, 4.815535977982682070 ) ) ;
#14647 = PLANE ( 'NONE',  #3466 ) ;
#14648 = CARTESIAN_POINT ( 'NONE',  ( 3.499999999999998668, -19.50000000000000000, 4.000000000000000000 ) ) ;
#14649 = VERTEX_POINT ( 'NONE', #17558 ) ;
#14650 = ORIENTED_EDGE ( 'NONE', *, *, #10142, .F. ) ;
#14651 = CARTESIAN_POINT ( 'NONE',  ( -12.00000000000000000, -25.49999999999998934, 1.000000000000000000 ) ) ;
#14652 = CARTESIAN_POINT ( 'NONE',  ( -11.00000000000000000, -24.49999999999999289, 5.000000000000000000 ) ) ;
#14653 = ADVANCED_FACE ( 'NONE', ( #6265 ), #10980, .T. ) ;
#14654 = FACE_OUTER_BOUND ( 'NONE', #18697, .T. ) ;
#14655 = AXIS2_PLACEMENT_3D ( 'NONE', #6939, #2133, #8514 ) ;
#14656 = LINE ( 'NONE', #11421, #2504 ) ;
#14657 = VECTOR ( 'NONE', #4987, 1000.000000000000000 ) ;
#14658 = VECTOR ( 'NONE', #295, 1000.000000000000000 ) ;
#14659 = DIRECTION ( 'NONE',  ( -1.000000000000000000, -1.192622389734054877E-16, 0.000000000000000000 ) ) ;
#14660 = CARTESIAN_POINT ( 'NONE',  ( -13.09293046926041626, 3.380488697651010011, 5.994170676248444352 ) ) ;
#14661 = CARTESIAN_POINT ( 'NONE',  ( 8.215308582316792396, -23.77099543870833998, 2.825813738724734847 ) ) ;
#14662 = VECTOR ( 'NONE', #1541, 1000.000000000000000 ) ;
#14663 = CARTESIAN_POINT ( 'NONE',  ( -4.999999999999998224, -2.500000000000047518, 9.999999999999998224 ) ) ;
#14664 = CARTESIAN_POINT ( 'NONE',  ( 13.10012427866737639, 3.743776072700027324, 6.001983176248468332 ) ) ;
#14665 = CARTESIAN_POINT ( 'NONE',  ( -2.731427961995660958, -10.89409100229510052, 2.829571171190552015 ) ) ;
#14666 = EDGE_LOOP ( 'NONE', ( #13613, #7833, #5186, #14803, #5949 ) ) ;
#14667 = CARTESIAN_POINT ( 'NONE',  ( -13.39662663169496781, -19.15785509940297615, 5.494950532956567102 ) ) ;
#14668 = CARTESIAN_POINT ( 'NONE',  ( 0.000000000000000000, 4.999999999999999112, 1.000000000000000000 ) ) ;
#14669 = CARTESIAN_POINT ( 'NONE',  ( 10.65969141768318096, -22.67418626127524917, 1.729004561291651809 ) ) ;
#14670 = CARTESIAN_POINT ( 'NONE',  ( -8.121558582316795949, -22.99999999999999645, 3.550687472877652073 ) ) ;
#14671 = ORIENTED_EDGE ( 'NONE', *, *, #16053, .F. ) ;
#14672 = CARTESIAN_POINT ( 'NONE',  ( 13.77324158252158171, -0.8888000826463379189, 6.637859435864801760 ) ) ;
#14673 = CARTESIAN_POINT ( 'NONE',  ( 13.12512971825177033, 5.006550771716304915, 5.133277049491872468 ) ) ;
#14674 = AXIS2_PLACEMENT_3D ( 'NONE', #9136, #10596, #1188 ) ;
#14675 = CARTESIAN_POINT ( 'NONE',  ( 17.12779268661489596, 0.000000000000000000, 1.000000000000000000 ) ) ;
#14676 = ORIENTED_EDGE ( 'NONE', *, *, #13121, .T. ) ;
#14677 = AXIS2_PLACEMENT_3D ( 'NONE', #6741, #3586, #9966 ) ;
#14678 = ORIENTED_EDGE ( 'NONE', *, *, #15141, .F. ) ;
#14679 = CARTESIAN_POINT ( 'NONE',  ( -27.00000000000000000, 0.000000000000000000, 1.000000000000000000 ) ) ;
#14680 = EDGE_CURVE ( 'NONE', #9626, #20665, #3334, .T. ) ;
#14681 = PLANE ( 'NONE',  #12241 ) ;
#14682 = DIRECTION ( 'NONE',  ( 0.000000000000000000, 1.000000000000000000, -0.000000000000000000 ) ) ;
#14683 = DIRECTION ( 'NONE',  ( 1.000000000000000000, 6.938893903907232322E-16, 0.000000000000000000 ) ) ;
#14684 = CARTESIAN_POINT ( 'NONE',  ( 1.939860967060266672, -10.52577007527361808, 2.542364016426418516 ) ) ;
#14685 = LINE ( 'NONE', #19612, #6393 ) ;
#14686 = VECTOR ( 'NONE', #3571, 1000.000000000000000 ) ;
#14687 = LINE ( 'NONE', #565, #11706 ) ;
#14688 = DIRECTION ( 'NONE',  ( 1.000000000000000000, 0.000000000000000000, -0.000000000000000000 ) ) ;
#14689 = LINE ( 'NONE', #568, #9641 ) ;
#14690 = CARTESIAN_POINT ( 'NONE',  ( -10.46530858231679417, -20.22900456129164937, 4.174186261275266929 ) ) ;
#14691 = CARTESIAN_POINT ( 'NONE',  ( -3.049989092406311109, -8.938202327316346896, 1.769874869409437279 ) ) ;
#14692 = ORIENTED_EDGE ( 'NONE', *, *, #1174, .T. ) ;
#14693 = CARTESIAN_POINT ( 'NONE',  ( -13.04243487821393721, 1.580461349787872782, 5.205428440007538349 ) ) ;
#14694 = CARTESIAN_POINT ( 'NONE',  ( -10.46530858231679417, -20.22900456129164937, 4.174186261275266929 ) ) ;
#14695 = VECTOR ( 'NONE', #2284, 1000.000000000000000 ) ;
#14696 = CARTESIAN_POINT ( 'NONE',  ( -7.565941417683176518, -23.20159541128344927, 2.226721677130534705 ) ) ;
#14697 = ORIENTED_EDGE ( 'NONE', *, *, #4062, .F. ) ;
#14698 = CARTESIAN_POINT ( 'NONE',  ( 13.84501469867711698, 4.235742283194553259, 4.583333333333295734 ) ) ;
#14699 = LINE ( 'NONE', #380, #16721 ) ;
#14700 = ORIENTED_EDGE ( 'NONE', *, *, #13882, .T. ) ;
#14701 = ORIENTED_EDGE ( 'NONE', *, *, #14872, .T. ) ;
#14702 = CARTESIAN_POINT ( 'NONE',  ( -21.42243175760212637, 9.000000000000001776, 0.000000000000000000 ) ) ;
#14703 = ORIENTED_EDGE ( 'NONE', *, *, #12843, .F. ) ;
#14704 = DIRECTION ( 'NONE',  ( -1.000000000000000000, -2.312964634635756072E-15, 0.000000000000000000 ) ) ;
#14705 = AXIS2_PLACEMENT_3D ( 'NONE', #7922, #1448, #3018 ) ;
#14706 = SHAPE_REPRESENTATION ( 'Cast Metal _ Plastic Body Housing', ( #18039 ), #14707 ) ;
#14707 =( GEOMETRIC_REPRESENTATION_CONTEXT ( 3 ) GLOBAL_UNCERTAINTY_ASSIGNED_CONTEXT ( ( #18648 ) ) GLOBAL_UNIT_ASSIGNED_CONTEXT ( ( #2200, #7021, #2506 ) ) REPRESENTATION_CONTEXT ( 'NONE', 'WORKASPACE' ) );
#14708 = VECTOR ( 'NONE', #13813, 1000.000000000000000 ) ;
#14709 = VERTEX_POINT ( 'NONE', #12746 ) ;
#14710 = CARTESIAN_POINT ( 'NONE',  ( 4.847191417683178294, -21.22443879296941915, 1.770995438708345748 ) ) ;
#14711 = DIRECTION ( 'NONE',  ( 1.000000000000000000, 0.000000000000000000, 0.000000000000000000 ) ) ;
#14712 = VECTOR ( 'NONE', #11614, 1000.000000000000000 ) ;
#14713 = EDGE_CURVE ( 'NONE', #11512, #8626, #7745, .T. ) ;
#14714 = CARTESIAN_POINT ( 'NONE',  ( -2.513306525444908512, -9.622685169956881168, 2.503048754562789746 ) ) ;
#14715 = CARTESIAN_POINT ( 'NONE',  ( 0.000000000000000000, 9.000000000000001776, 0.000000000000000000 ) ) ;
#14716 = CARTESIAN_POINT ( 'NONE',  ( -5.590308582316794173, -21.32581373872472952, 1.729004561291657138 ) ) ;
#14717 = EDGE_CURVE ( 'NONE', #19171, #20470, #3233, .T. ) ;
#14718 = CARTESIAN_POINT ( 'NONE',  ( 8.878441417683177406, -23.74999999999999645, 3.449312527122335492 ) ) ;
#14719 = CARTESIAN_POINT ( 'NONE',  ( 13.42791111847407848, 9.000000000000001776, 1.000000000000000000 ) ) ;
#14720 = CARTESIAN_POINT ( 'NONE',  ( -6.534691417683176518, -20.22900456129164581, 2.825813738724747726 ) ) ;
#14721 = VERTEX_POINT ( 'NONE', #4591 ) ;
#14722 = CARTESIAN_POINT ( 'NONE',  ( 12.99655858231679595, -22.05068747287764452, 0.9999999999999978906 ) ) ;
#14723 = CARTESIAN_POINT ( 'NONE',  ( 12.64691428603184242, -19.14332855539073464, 5.509795676248469221 ) ) ;
#14724 = CARTESIAN_POINT ( 'NONE',  ( -13.15498530132288479, 5.764257716805535559, 4.583333333333295734 ) ) ;
#14725 = AXIS2_PLACEMENT_3D ( 'NONE', #18104, #8478, #2094 ) ;
#14726 = ORIENTED_EDGE ( 'NONE', *, *, #5440, .F. ) ;
#14727 = VECTOR ( 'NONE', #5707, 1000.000000000000000 ) ;
#14728 = VECTOR ( 'NONE', #4741, 1000.000000000000000 ) ;
#14729 = LINE ( 'NONE', #3539, #17637 ) ;
#14730 = DIRECTION ( 'NONE',  ( 1.000000000000000000, 0.000000000000000000, 0.000000000000000000 ) ) ;
#14731 = VECTOR ( 'NONE', #9850, 1000.000000000000000 ) ;
#14732 = VERTEX_POINT ( 'NONE', #9604 ) ;
#14733 = PRODUCT_CONTEXT ( 'NONE', #15087, 'mechanical' ) ;
#14734 = ORIENTED_EDGE ( 'NONE', *, *, #8922, .F. ) ;
#14735 = DIRECTION ( 'NONE',  ( 1.000000000000000000, 0.000000000000000000, -0.000000000000000000 ) ) ;
#14736 = ORIENTED_EDGE ( 'NONE', *, *, #959, .T. ) ;
#14737 = CARTESIAN_POINT ( 'NONE',  ( 0.000000000000000000, 16.00000000000000000, 1.000000000000000000 ) ) ;
#14738 = CARTESIAN_POINT ( 'NONE',  ( 12.66849571425264287, -18.05346643024382303, 5.533233176248494978 ) ) ;
#14739 = EDGE_CURVE ( 'NONE', #18649, #2409, #18963, .T. ) ;
#14740 = CARTESIAN_POINT ( 'NONE',  ( 0.000000000000000000, 4.999999999999999112, 1.000000000000000000 ) ) ;
#14741 = VECTOR ( 'NONE', #19078, 1000.000000000000000 ) ;
#14742 = CARTESIAN_POINT ( 'NONE',  ( 12.62515553039088090, -20.24214571525854467, 4.629702272822510345 ) ) ;
#14743 = LINE ( 'NONE', #3763, #13683 ) ;
#14744 = CARTESIAN_POINT ( 'NONE',  ( -13.37499999999998224, -20.24999999999991829, 4.333333333333343695 ) ) ;
#14745 = CARTESIAN_POINT ( 'NONE',  ( 11.02780858231679595, -24.47900456129166358, 4.586221378810390270 ) ) ;
#14746 = CARTESIAN_POINT ( 'NONE',  ( -13.15384296923648400, 5.706569946443514674, 5.461568745250741763 ) ) ;
#14747 = CARTESIAN_POINT ( 'NONE',  ( -4.934058582316795061, -23.73192549717337130, 5.303608408759367343 ) ) ;
#14748 = DIRECTION ( 'NONE',  ( -6.938893903907222067E-15, 1.000000000000000000, 0.000000000000000000 ) ) ;
#14749 = LINE ( 'NONE', #3660, #16753 ) ;
#14750 = CARTESIAN_POINT ( 'NONE',  ( 11.30905858231679595, -22.74294823697954016, 2.828734674606448785 ) ) ;
#14751 = CARTESIAN_POINT ( 'NONE',  ( -9.909691417683179182, -21.32581373872474373, 5.270995438708348857 ) ) ;
#14752 = ORIENTED_EDGE ( 'NONE', *, *, #17333, .F. ) ;
#14753 = VERTEX_POINT ( 'NONE', #4900 ) ;
#14754 = CARTESIAN_POINT ( 'NONE',  ( 13.83770801678722329, 3.866754847752558621, 5.240062463382368030 ) ) ;
#14755 = CARTESIAN_POINT ( 'NONE',  ( 11.00000000000000000, -25.49999999999999645, 6.500000000000000000 ) ) ;
#14756 = CARTESIAN_POINT ( 'NONE',  ( -17.94064177244175795, 16.00000000000000000, 1.000000000000000000 ) ) ;
#14757 = VERTEX_POINT ( 'NONE', #17660 ) ;
#14758 = VECTOR ( 'NONE', #12326, 1000.000000000000000 ) ;
#14759 = CARTESIAN_POINT ( 'NONE',  ( 14.50000000000001243, -18.49999999999999645, 4.000000000000000000 ) ) ;
#14760 = CARTESIAN_POINT ( 'NONE',  ( -7.500000000000000000, -24.49999999999999289, 5.000000000000000000 ) ) ;
#14761 = CARTESIAN_POINT ( 'NONE',  ( 13.37883250981221472, -20.05645825448334563, 5.102688967256983510 ) ) ;
#14762 = EDGE_CURVE ( 'NONE', #8919, #7660, #20516, .T. ) ;
#14763 = EDGE_CURVE ( 'NONE', #15727, #8843, #3648, .T. ) ;
#14764 = DIRECTION ( 'NONE',  ( 0.000000000000000000, 1.000000000000000000, -0.000000000000000000 ) ) ;
#14765 = CARTESIAN_POINT ( 'NONE',  ( 3.996922828336520794, -14.62728872172488437, 3.980945906412841850 ) ) ;
#14766 = CARTESIAN_POINT ( 'NONE',  ( 1.948765222931501784, -9.143197003266354983, 1.629906614618163552 ) ) ;
#14767 = CARTESIAN_POINT ( 'NONE',  ( -12.62499994688180749, -19.50000268246798640, 4.473800639250938183 ) ) ;
#14768 = CARTESIAN_POINT ( 'NONE',  ( 9.152808582316794173, -21.22443879296942626, 5.229004561291660025 ) ) ;
#14769 = CARTESIAN_POINT ( 'NONE',  ( 19.23630159782011617, 9.000000000000001776, 1.000000000000000000 ) ) ;
#14770 = CARTESIAN_POINT ( 'NONE',  ( 12.62503117662529739, -20.24842558042254836, 4.565011198945062354 ) ) ;
#14771 = AXIS2_PLACEMENT_3D ( 'NONE', #11470, #17852, #6352 ) ;
#14772 = CARTESIAN_POINT ( 'NONE',  ( -0.9854920305337622199, -9.864917468222230923, 2.372643865078341019 ) ) ;
#14773 = CARTESIAN_POINT ( 'NONE',  ( 21.25349085826861995, 0.000000000000000000, 1.000000000000000000 ) ) ;
#14774 = EDGE_CURVE ( 'NONE', #13772, #10231, #10276, .T. ) ;
#14775 = CARTESIAN_POINT ( 'NONE',  ( 6.159691417683176518, -22.67418626127524917, 1.729004561291651809 ) ) ;
#14776 = CARTESIAN_POINT ( 'NONE',  ( -7.465308582316796837, -20.97900456129165647, 3.863526089495444626 ) ) ;
#14777 = EDGE_LOOP ( 'NONE', ( #12234, #1438, #10015, #2220 ) ) ;
#14778 = CARTESIAN_POINT ( 'NONE',  ( 13.86676110481170632, 3.833935792988865110, 6.739421935864088553 ) ) ;
#14779 = CARTESIAN_POINT ( 'NONE',  ( 12.65650603190776025, -18.65894538865861563, 5.520212342915047365 ) ) ;
#14780 = CARTESIAN_POINT ( 'NONE',  ( 7.619520639128047002, 4.999999999999999112, 1.000000000000000000 ) ) ;
#14781 = VERTEX_POINT ( 'NONE', #13470 ) ;
#14782 = ORIENTED_EDGE ( 'NONE', *, *, #18958, .T. ) ;
#14783 = CARTESIAN_POINT ( 'NONE',  ( 8.119520639128047890, 0.000000000000000000, 1.000000000000000000 ) ) ;
#14784 = AXIS2_PLACEMENT_3D ( 'NONE', #1898, #14856, #16528 ) ;
#14785 = LINE ( 'NONE', #5576, #3897 ) ;
#14786 = EDGE_CURVE ( 'NONE', #13894, #13945, #6259, .T. ) ;
#14787 = ADVANCED_FACE ( 'NONE', ( #13163 ), #10030, .F. ) ;
#14788 = PLANE ( 'NONE',  #7322 ) ;
#14789 = DIRECTION ( 'NONE',  ( 0.000000000000000000, -1.000000000000000000, 0.000000000000000000 ) ) ;
#14790 = CARTESIAN_POINT ( 'NONE',  ( 2.067263844777544435, -10.27417889452513933, 1.727750375171331676 ) ) ;
#14791 = CARTESIAN_POINT ( 'NONE',  ( 15.86404127825609400, 0.000000000000000000, 1.000000000000000000 ) ) ;
#14792 = PLANE ( 'NONE',  #13393 ) ;
#14793 = CARTESIAN_POINT ( 'NONE',  ( 12.70105350217228413, -20.47677344150786283, 3.540713189489502977 ) ) ;
#14794 = LINE ( 'NONE', #16363, #5296 ) ;
#14795 = CARTESIAN_POINT ( 'NONE',  ( -10.65280858231679240, -21.22443879296942626, 5.229004561291659137 ) ) ;
#14796 = CARTESIAN_POINT ( 'NONE',  ( -0.2815691515810352374, -8.364917468222230923, 2.372643865078523540 ) ) ;
#14797 = VERTEX_POINT ( 'NONE', #2386 ) ;
#14798 = CARTESIAN_POINT ( 'NONE',  ( -12.65396917024039958, -18.03705690286155772, 4.783553440007634272 ) ) ;
#14799 = CARTESIAN_POINT ( 'NONE',  ( -8.121558582316792396, -23.74999999999999645, 3.550687472877651629 ) ) ;
#14800 = VECTOR ( 'NONE', #14113, 1000.000000000000000 ) ;
#14801 = EDGE_CURVE ( 'NONE', #15169, #17122, #11599, .T. ) ;
#14802 = CARTESIAN_POINT ( 'NONE',  ( -6.065941417683177406, -23.20159541128344927, 2.226721677130534705 ) ) ;
#14803 = ORIENTED_EDGE ( 'NONE', *, *, #18103, .F. ) ;
#14804 = CARTESIAN_POINT ( 'NONE',  ( 13.83890698502169059, 3.927302743594121903, 5.241364546715693074 ) ) ;
#14805 = LINE ( 'NONE', #6764, #4371 ) ;
#14806 = VERTEX_POINT ( 'NONE', #11594 ) ;
#14807 = ORIENTED_EDGE ( 'NONE', *, *, #18303, .T. ) ;
#14808 = CARTESIAN_POINT ( 'NONE',  ( 11.00000000000000000, -24.49999999999999289, 4.000000000000000000 ) ) ;
#14809 = VERTEX_POINT ( 'NONE', #1978 ) ;
#14810 = CARTESIAN_POINT ( 'NONE',  ( 13.92791111847407848, 0.000000000000000000, 0.000000000000000000 ) ) ;
#14811 = AXIS2_PLACEMENT_3D ( 'NONE', #17781, #107, #6493 ) ;
#14812 = ORIENTED_EDGE ( 'NONE', *, *, #9606, .T. ) ;
#14813 = CARTESIAN_POINT ( 'NONE',  ( 7.472191417683176518, -23.72900456129164937, 2.724438792969417378 ) ) ;
#14814 = LINE ( 'NONE', #2255, #15657 ) ;
#14815 = DIRECTION ( 'NONE',  ( -0.000000000000000000, -0.000000000000000000, -1.000000000000000000 ) ) ;
#14816 = DIRECTION ( 'NONE',  ( 1.000000000000000000, 0.000000000000000000, 0.000000000000000000 ) ) ;
#14817 = FACE_OUTER_BOUND ( 'NONE', #6709, .T. ) ;
#14818 = DIRECTION ( 'NONE',  ( 0.000000000000000000, 1.000000000000000000, -0.000000000000000000 ) ) ;
#14819 = CARTESIAN_POINT ( 'NONE',  ( 7.659691417683177406, -22.67418626127524917, 1.729004561291651809 ) ) ;
#14820 = DIRECTION ( 'NONE',  ( -1.000000000000000000, -0.000000000000000000, -0.000000000000000000 ) ) ;
#14821 = CARTESIAN_POINT ( 'NONE',  ( -11.31594141768317741, -21.32873467460645145, 4.242948236979555254 ) ) ;
#14822 = CARTESIAN_POINT ( 'NONE',  ( -9.902808582316795949, -23.08622137881038938, 1.020995438708339309 ) ) ;
#14823 = EDGE_LOOP ( 'NONE', ( #8610, #8132 ) ) ;
#14824 = CARTESIAN_POINT ( 'NONE',  ( 12.63465172146706728, -19.76258806590802664, 5.372658420469845986 ) ) ;
#14826 = CARTESIAN_POINT ( 'NONE',  ( -13.10026320386584153, 3.000791795219782454, 6.736037912489353019 ) ) ;
#14825 = VECTOR ( 'NONE', #6271, 1000.000000000000000 ) ;
#14827 = ORIENTED_EDGE ( 'NONE', *, *, #16551, .F. ) ;
#14828 = EDGE_CURVE ( 'NONE', #2248, #6861, #17977, .T. ) ;
#14829 = CARTESIAN_POINT ( 'NONE',  ( 1.811130159782011528, 9.000000000000001776, 1.000000000000000000 ) ) ;
#14830 = LINE ( 'NONE', #7201, #9333 ) ;
#14831 =( BOUNDED_SURFACE ( )  B_SPLINE_SURFACE ( 3, 2, ( 
 ( #1932, #4658, #11050, #1524, #4764, #4864, #15846, #7904, #11149, #16170, #3293, #17518, #17738, #11244, #8006, #14268, #3403, #3199, #14582, #1625, #14378, #16063, #6448, #8118, #163, #9783, #1833, #257, #3712, #14795, #4018, #14690, #6950, #7061, #11650, #5484, #5381, #11553, #7165, #16774, #8623, #18249, #5274, #9981, #569, #3813, #371, #19521, #474, #5173, #17933, #18148, #19831, #10403, #13425, #13124, #3602, #2140, #16561, #16364, #10092, #2443, #11857, #10191, #6755, #2040, #18041, #8428, #10292, #14993, #674, #6848, #2236, #13217, #19616, #18353, #3912, #16662, #16467, #8522, #19930, #13528, #13320, #14891, #19721, #15102, #2340, #5587, #11757, #8734, #779, #11958, #2651, #18872, #10711 ),
 ( #1293, #10918, #2763, #12376, #20138, #4122, #17185, #879, #4533, #9141, #9238, #7474, #16975, #5798, #8835, #7672, #7263, #1094, #9039, #18660, #15610, #6109, #14042, #10503, #20452, #4221, #4436, #18459, #17280, #18770, #13624, #4328, #13934, #2863, #15302, #12479, #15203, #12069, #5896, #7572, #20032, #16873, #2543, #5694, #15411, #10601, #13833, #8931, #12169, #981, #7370, #20238, #13734, #18557, #12266, #17085, #15511, #1193, #20337, #6001, #10820, #8267, #14844, #3554, #7879, #5331, #6803, #8374, #6204, #8477, #5224, #11022, #11507, #15717, #19080, #11705, #16314, #13073, #2965, #12573, #6305, #18974, #19571, #17887, #9935, #9341, #6702, #15820, #17391, #6900, #14747, #1987, #4628, #3074, #519 ),
 ( #5022, #3657, #424, #13268, #1401, #9449, #13171, #11402, #17787, #19667, #5127, #14146, #12677, #1498, #11602, #3455, #17987, #9833, #10040, #7783, #16417, #20553, #14239, #2093, #16218, #20646, #1887, #14633, #318, #19473, #18298, #7008, #4073, #7215, #18201, #3766, #10146, #10459, #13577, #830, #16925, #18409, #5853, #8788, #12013, #11908, #3961, #8573, #5752, #20086, #19779, #15048, #10241, #14943, #3864, #621, #18101, #2397, #10556, #10349, #2287, #7317, #19979, #8885, #16607, #15254, #13479, #5640, #12122, #20193, #18514, #8678, #15360, #4175, #16828, #931, #7426, #13678, #733, #2599, #13377, #5437, #13788, #7116, #16517, #19882, #8987, #2189, #16722, #2492, #11810, #5538, #15156, #1041, #2711 ),
 ( #4583, #10659, #9093, #20398, #14098, #15463, #7926, #6061, #20291, #1248, #4487, #4686, #7622, #12321, #1548, #12223, #10872, #10971, #9190, #3024, #2916, #1148, #11077, #14293, #6160, #15772, #2816, #7525, #20601, #4273, #20704, #12528, #12627, #17237, #12430, #15565, #18612, #17448, #17033, #9293, #18825, #1352, #19031, #9500, #3126, #13889, #15872, #13990, #7832, #5948, #18719, #1453, #4386, #7733, #17341, #6253, #10769, #17137, #15668, #20507, #18925, #9400, #14194, #15973, #9595, #14720, #14511, #8147, #188, #6367, #9705, #19140, #12736, #17763, #2069, #6476, #8039, #4791, #14405, #8243, #11483, #17863, #11374, #3432, #17960, #6677, #11269, #8454, #9909, #3533, #1655, #11580, #8344, #90, #14608 ),
 ( #11173, #12836, #17547, #3224, #9809, #16290, #16391, #19446, #19239, #4889, #6570, #286, #17650, #1761, #14821, #5104, #16196, #3323, #16091, #12935, #19340, #1961, #13046, #397, #4995, #1861, #6780, #13150, #10012, #19547, #5202, #3631, #597, #5729, #13654, #18176, #13352, #18073, #6983, #3739, #496, #5512, #20065, #7090, #5410, #10434, #16695, #11990, #19752, #18388, #16586, #2373, #2472, #2574, #8863, #11784, #18490, #15232, #3938, #4051, #10534, #16804, #3838, #906, #10121, #16493, #16903, #10218, #19643, #2263, #7291, #6876, #13455, #10326, #13245, #5302, #8652, #11676, #2165, #8762, #5614, #8959, #13555, #8549, #14919, #15024, #15134, #705, #19859, #11884, #19956, #808, #18276, #7192, #12100 ),
 ( #4152, #15334, #18802, #7506, #9072, #19007, #6139, #14075, #17009, #15444, #20581, #7812, #13968, #4663, #10745, #15749, #1331, #6234, #1014, #2686, #2894, #17115, #9171, #11054, #17216, #5830, #18695, #4252, #20483, #15546, #12508, #4361, #3000, #17427, #18906, #7405, #3103, #9375, #7602, #13766, #2797, #20170, #12199, #12604, #1226, #10632, #7707, #4468, #1128, #18589, #13869, #4563, #10853, #9270, #14174, #15643, #20269, #6036, #10948, #20373, #12408, #5927, #1431, #17314, #12298, #11153, #6452, #1630, #6342, #15948, #12713, #9480, #14489, #1936, #16067, #14383, #19425, #4972, #261, #8010, #6652, #4869, #11351, #11458, #11557, #17842, #66, #6759, #3507, #12913, #13022, #19525, #5082, #12816, #9888 ),
 ( #19215, #7908, #11248, #16268, #15850, #1740, #19316, #1529, #14272, #17627, #20679, #19116, #17742, #14586, #5178, #1838, #4768, #17523, #3299, #3406, #3204, #9681, #17938, #8223, #9788, #9575, #8122, #166, #6549, #8320, #16174, #14694, #376, #13128, #16471, #18046, #7268, #15107, #2344, #5278, #3718, #8839, #16779, #2240, #13628, #19725, #4022, #10296, #15207, #9987, #11654, #11861, #5386, #18152, #20037, #5488, #14799, #6954, #13223, #8738, #3817, #783, #13326, #11962, #5699, #7169, #16368, #12073, #18359, #16565, #2047, #11761, #8432, #3606, #883, #10195, #19620, #16668, #13430, #10096, #478, #6852, #13532, #19835, #7066, #2447, #3916, #2144, #14998, #18254, #8628, #679, #8526, #10407, #5591 ) ),
 .UNSPECIFIED., .T., .F., .F. ) 
 B_SPLINE_SURFACE_WITH_KNOTS ( ( 4, 3, 4 ),
 ( 3, 2, 2, 2, 2, 2, 2, 2, 2, 2, 2, 2, 2, 2, 2, 2, 2, 2, 2, 2, 2, 2, 2, 2, 2, 2, 2, 2, 2, 2, 2, 2, 2, 2, 2, 2, 2, 2, 2, 2, 2, 2, 2, 2, 2, 2, 2, 3 ),
 ( 0.000000000000000000, 0.5000000000000000000, 1.000000000000000000 ),
 ( 0.000000000000000000, 0.02083333333333333218, 0.04166666666666666435, 0.06250000000000000000, 0.08333333333333332871, 0.1041666666666666713, 0.1250000000000000000, 0.1458333333333333426, 0.1666666666666666574, 0.1875000000000000000, 0.2083333333333333426, 0.2291666666666666574, 0.2500000000000000000, 0.2708333333333333148, 0.2916666666666666852, 0.3125000000000000000, 0.3333333333333333148, 0.3541666666666666852, 0.3750000000000000000, 0.3958333333333333148, 0.4166666666666666852, 0.4375000000000000000, 0.4583333333333333148, 0.4791666666666666852, 0.5000000000000000000, 0.5208333333333333703, 0.5416666666666666297, 0.5625000000000000000, 0.5833333333333333703, 0.6041666666666666297, 0.6250000000000000000, 0.6458333333333333703, 0.6666666666666666297, 0.6875000000000000000, 0.7083333333333333703, 0.7291666666666666297, 0.7500000000000000000, 0.7708333333333333703, 0.7916666666666666297, 0.8125000000000000000, 0.8333333333333333703, 0.8541666666666666297, 0.8750000000000000000, 0.8958333333333333703, 0.9166666666666666297, 0.9375000000000000000, 0.9583333333333333703, 0.9650437087885355147 ),
 .UNSPECIFIED. ) 
 GEOMETRIC_REPRESENTATION_ITEM ( )  RATIONAL_B_SPLINE_SURFACE ( (
 ( 1.000000000000000000, 0.9238795325112867385, 1.000000000000000000, 0.9238795325112867385, 1.000000000000000000, 0.9238795325112867385, 1.000000000000000000, 0.9238795325112867385, 1.000000000000000000, 0.9238795325112867385, 1.000000000000000000, 0.9238795325112867385, 1.000000000000000000, 0.9238795325112867385, 1.000000000000000000, 0.9238795325112867385, 1.000000000000000000, 0.9238795325112867385, 1.000000000000000000, 0.9238795325112867385, 1.000000000000000000, 0.9238795325112867385, 1.000000000000000000, 0.9238795325112867385, 1.000000000000000000, 0.9238795325112867385, 1.000000000000000000, 0.9238795325112867385, 1.000000000000000000, 0.9238795325112867385, 1.000000000000000000, 0.9238795325112867385, 1.000000000000000000, 0.9238795325112867385, 1.000000000000000000, 0.9238795325112867385, 1.000000000000000000, 0.9238795325112867385, 1.000000000000000000, 0.9238795325112867385, 1.000000000000000000, 0.9238795325112867385, 1.000000000000000000, 0.9238795325112867385, 1.000000000000000000, 0.9238795325112867385, 1.000000000000000000, 0.9238795325112867385, 1.000000000000000000, 0.9238795325112867385, 1.000000000000000000, 0.9238795325112867385, 1.000000000000000000, 0.9238795325112867385, 1.000000000000000000, 0.9238795325112867385, 1.000000000000000000, 0.9238795325112867385, 1.000000000000000000, 0.9238795325112867385, 1.000000000000000000, 0.9238795325112867385, 1.000000000000000000, 0.9238795325112867385, 1.000000000000000000, 0.9238795325112867385, 1.000000000000000000, 0.9238795325112867385, 1.000000000000000000, 0.9238795325112867385, 1.000000000000000000, 0.9238795325112867385, 1.000000000000000000, 0.9238795325112867385, 1.000000000000000000, 0.9238795325112867385, 1.000000000000000000, 0.9238795325112867385, 1.000000000000000000, 0.9238795325112867385, 1.000000000000000000, 0.9238795325112867385, 1.000000000000000000, 0.9238795325112867385, 1.000000000000000000, 0.9238795325112867385, 1.000000000000000000, 0.9238795325112867385, 1.000000000000000000, 0.9238795325112867385, 1.000000000000000000, 0.9238795325112867385, 1.000000000000000000, 0.9754817479996107377, 0.9667580569362973497),
 ( 0.3333333333333333703, 0.3079598441704289313, 0.3333333333333333703, 0.3079598441704289313, 0.3333333333333333703, 0.3079598441704289313, 0.3333333333333333703, 0.3079598441704289313, 0.3333333333333333703, 0.3079598441704289313, 0.3333333333333333703, 0.3079598441704289313, 0.3333333333333333703, 0.3079598441704289313, 0.3333333333333333703, 0.3079598441704289313, 0.3333333333333333703, 0.3079598441704289313, 0.3333333333333333703, 0.3079598441704289313, 0.3333333333333333703, 0.3079598441704289313, 0.3333333333333333703, 0.3079598441704289313, 0.3333333333333333703, 0.3079598441704289313, 0.3333333333333333703, 0.3079598441704289313, 0.3333333333333333703, 0.3079598441704289313, 0.3333333333333333703, 0.3079598441704289313, 0.3333333333333333703, 0.3079598441704289313, 0.3333333333333333703, 0.3079598441704289313, 0.3333333333333333703, 0.3079598441704289313, 0.3333333333333333703, 0.3079598441704289313, 0.3333333333333333703, 0.3079598441704289313, 0.3333333333333333703, 0.3079598441704289313, 0.3333333333333333703, 0.3079598441704289313, 0.3333333333333333703, 0.3079598441704289313, 0.3333333333333333703, 0.3079598441704289313, 0.3333333333333333703, 0.3079598441704289313, 0.3333333333333333703, 0.3079598441704289313, 0.3333333333333333703, 0.3079598441704289313, 0.3333333333333333703, 0.3079598441704289313, 0.3333333333333333703, 0.3079598441704289313, 0.3333333333333333703, 0.3079598441704289313, 0.3333333333333333703, 0.3079598441704289313, 0.3333333333333333703, 0.3079598441704289313, 0.3333333333333333703, 0.3079598441704289313, 0.3333333333333333703, 0.3079598441704289313, 0.3333333333333333703, 0.3079598441704289313, 0.3333333333333333703, 0.3079598441704289313, 0.3333333333333333703, 0.3079598441704289313, 0.3333333333333333703, 0.3079598441704289313, 0.3333333333333333703, 0.3079598441704289313, 0.3333333333333333703, 0.3079598441704289313, 0.3333333333333333703, 0.3079598441704289313, 0.3333333333333333703, 0.3079598441704289313, 0.3333333333333333703, 0.3079598441704289313, 0.3333333333333333703, 0.3079598441704289313, 0.3333333333333333703, 0.3079598441704289313, 0.3333333333333333703, 0.3251605826665369681, 0.3222526856454325239),
 ( 0.3333333333333333703, 0.3079598441704289313, 0.3333333333333333703, 0.3079598441704289313, 0.3333333333333333703, 0.3079598441704289313, 0.3333333333333333703, 0.3079598441704289313, 0.3333333333333333703, 0.3079598441704289313, 0.3333333333333333703, 0.3079598441704289313, 0.3333333333333333703, 0.3079598441704289313, 0.3333333333333333703, 0.3079598441704289313, 0.3333333333333333703, 0.3079598441704289313, 0.3333333333333333703, 0.3079598441704289313, 0.3333333333333333703, 0.3079598441704289313, 0.3333333333333333703, 0.3079598441704289313, 0.3333333333333333703, 0.3079598441704289313, 0.3333333333333333703, 0.3079598441704289313, 0.3333333333333333703, 0.3079598441704289313, 0.3333333333333333703, 0.3079598441704289313, 0.3333333333333333703, 0.3079598441704289313, 0.3333333333333333703, 0.3079598441704289313, 0.3333333333333333703, 0.3079598441704289313, 0.3333333333333333703, 0.3079598441704289313, 0.3333333333333333703, 0.3079598441704289313, 0.3333333333333333703, 0.3079598441704289313, 0.3333333333333333703, 0.3079598441704289313, 0.3333333333333333703, 0.3079598441704289313, 0.3333333333333333703, 0.3079598441704289313, 0.3333333333333333703, 0.3079598441704289313, 0.3333333333333333703, 0.3079598441704289313, 0.3333333333333333703, 0.3079598441704289313, 0.3333333333333333703, 0.3079598441704289313, 0.3333333333333333703, 0.3079598441704289313, 0.3333333333333333703, 0.3079598441704289313, 0.3333333333333333703, 0.3079598441704289313, 0.3333333333333333703, 0.3079598441704289313, 0.3333333333333333703, 0.3079598441704289313, 0.3333333333333333703, 0.3079598441704289313, 0.3333333333333333703, 0.3079598441704289313, 0.3333333333333333703, 0.3079598441704289313, 0.3333333333333333703, 0.3079598441704289313, 0.3333333333333333703, 0.3079598441704289313, 0.3333333333333333703, 0.3079598441704289313, 0.3333333333333333703, 0.3079598441704289313, 0.3333333333333333703, 0.3079598441704289313, 0.3333333333333333703, 0.3079598441704289313, 0.3333333333333333703, 0.3079598441704289313, 0.3333333333333333703, 0.3079598441704289313, 0.3333333333333333703, 0.3079598441704289313, 0.3333333333333333703, 0.3251605826665369681, 0.3222526856454325239),
 ( 1.000000000000000000, 0.9238795325112867385, 1.000000000000000000, 0.9238795325112867385, 1.000000000000000000, 0.9238795325112867385, 1.000000000000000000, 0.9238795325112867385, 1.000000000000000000, 0.9238795325112867385, 1.000000000000000000, 0.9238795325112867385, 1.000000000000000000, 0.9238795325112867385, 1.000000000000000000, 0.9238795325112867385, 1.000000000000000000, 0.9238795325112867385, 1.000000000000000000, 0.9238795325112867385, 1.000000000000000000, 0.9238795325112867385, 1.000000000000000000, 0.9238795325112867385, 1.000000000000000000, 0.9238795325112867385, 1.000000000000000000, 0.9238795325112867385, 1.000000000000000000, 0.9238795325112867385, 1.000000000000000000, 0.9238795325112867385, 1.000000000000000000, 0.9238795325112867385, 1.000000000000000000, 0.9238795325112867385, 1.000000000000000000, 0.9238795325112867385, 1.000000000000000000, 0.9238795325112867385, 1.000000000000000000, 0.9238795325112867385, 1.000000000000000000, 0.9238795325112867385, 1.000000000000000000, 0.9238795325112867385, 1.000000000000000000, 0.9238795325112867385, 1.000000000000000000, 0.9238795325112867385, 1.000000000000000000, 0.9238795325112867385, 1.000000000000000000, 0.9238795325112867385, 1.000000000000000000, 0.9238795325112867385, 1.000000000000000000, 0.9238795325112867385, 1.000000000000000000, 0.9238795325112867385, 1.000000000000000000, 0.9238795325112867385, 1.000000000000000000, 0.9238795325112867385, 1.000000000000000000, 0.9238795325112867385, 1.000000000000000000, 0.9238795325112867385, 1.000000000000000000, 0.9238795325112867385, 1.000000000000000000, 0.9238795325112867385, 1.000000000000000000, 0.9238795325112867385, 1.000000000000000000, 0.9238795325112867385, 1.000000000000000000, 0.9238795325112867385, 1.000000000000000000, 0.9238795325112867385, 1.000000000000000000, 0.9238795325112867385, 1.000000000000000000, 0.9238795325112867385, 1.000000000000000000, 0.9238795325112867385, 1.000000000000000000, 0.9238795325112867385, 1.000000000000000000, 0.9238795325112867385, 1.000000000000000000, 0.9238795325112867385, 1.000000000000000000, 0.9754817479996107377, 0.9667580569362973497),
 ( 0.3333333333333333703, 0.3079598441704289313, 0.3333333333333333703, 0.3079598441704289313, 0.3333333333333333703, 0.3079598441704289313, 0.3333333333333333703, 0.3079598441704289313, 0.3333333333333333703, 0.3079598441704289313, 0.3333333333333333703, 0.3079598441704289313, 0.3333333333333333703, 0.3079598441704289313, 0.3333333333333333703, 0.3079598441704289313, 0.3333333333333333703, 0.3079598441704289313, 0.3333333333333333703, 0.3079598441704289313, 0.3333333333333333703, 0.3079598441704289313, 0.3333333333333333703, 0.3079598441704289313, 0.3333333333333333703, 0.3079598441704289313, 0.3333333333333333703, 0.3079598441704289313, 0.3333333333333333703, 0.3079598441704289313, 0.3333333333333333703, 0.3079598441704289313, 0.3333333333333333703, 0.3079598441704289313, 0.3333333333333333703, 0.3079598441704289313, 0.3333333333333333703, 0.3079598441704289313, 0.3333333333333333703, 0.3079598441704289313, 0.3333333333333333703, 0.3079598441704289313, 0.3333333333333333703, 0.3079598441704289313, 0.3333333333333333703, 0.3079598441704289313, 0.3333333333333333703, 0.3079598441704289313, 0.3333333333333333703, 0.3079598441704289313, 0.3333333333333333703, 0.3079598441704289313, 0.3333333333333333703, 0.3079598441704289313, 0.3333333333333333703, 0.3079598441704289313, 0.3333333333333333703, 0.3079598441704289313, 0.3333333333333333703, 0.3079598441704289313, 0.3333333333333333703, 0.3079598441704289313, 0.3333333333333333703, 0.3079598441704289313, 0.3333333333333333703, 0.3079598441704289313, 0.3333333333333333703, 0.3079598441704289313, 0.3333333333333333703, 0.3079598441704289313, 0.3333333333333333703, 0.3079598441704289313, 0.3333333333333333703, 0.3079598441704289313, 0.3333333333333333703, 0.3079598441704289313, 0.3333333333333333703, 0.3079598441704289313, 0.3333333333333333703, 0.3079598441704289313, 0.3333333333333333703, 0.3079598441704289313, 0.3333333333333333703, 0.3079598441704289313, 0.3333333333333333703, 0.3079598441704289313, 0.3333333333333333703, 0.3079598441704289313, 0.3333333333333333703, 0.3079598441704289313, 0.3333333333333333703, 0.3079598441704289313, 0.3333333333333333703, 0.3251605826665369681, 0.3222526856454325239),
 ( 0.3333333333333333703, 0.3079598441704289313, 0.3333333333333333703, 0.3079598441704289313, 0.3333333333333333703, 0.3079598441704289313, 0.3333333333333333703, 0.3079598441704289313, 0.3333333333333333703, 0.3079598441704289313, 0.3333333333333333703, 0.3079598441704289313, 0.3333333333333333703, 0.3079598441704289313, 0.3333333333333333703, 0.3079598441704289313, 0.3333333333333333703, 0.3079598441704289313, 0.3333333333333333703, 0.3079598441704289313, 0.3333333333333333703, 0.3079598441704289313, 0.3333333333333333703, 0.3079598441704289313, 0.3333333333333333703, 0.3079598441704289313, 0.3333333333333333703, 0.3079598441704289313, 0.3333333333333333703, 0.3079598441704289313, 0.3333333333333333703, 0.3079598441704289313, 0.3333333333333333703, 0.3079598441704289313, 0.3333333333333333703, 0.3079598441704289313, 0.3333333333333333703, 0.3079598441704289313, 0.3333333333333333703, 0.3079598441704289313, 0.3333333333333333703, 0.3079598441704289313, 0.3333333333333333703, 0.3079598441704289313, 0.3333333333333333703, 0.3079598441704289313, 0.3333333333333333703, 0.3079598441704289313, 0.3333333333333333703, 0.3079598441704289313, 0.3333333333333333703, 0.3079598441704289313, 0.3333333333333333703, 0.3079598441704289313, 0.3333333333333333703, 0.3079598441704289313, 0.3333333333333333703, 0.3079598441704289313, 0.3333333333333333703, 0.3079598441704289313, 0.3333333333333333703, 0.3079598441704289313, 0.3333333333333333703, 0.3079598441704289313, 0.3333333333333333703, 0.3079598441704289313, 0.3333333333333333703, 0.3079598441704289313, 0.3333333333333333703, 0.3079598441704289313, 0.3333333333333333703, 0.3079598441704289313, 0.3333333333333333703, 0.3079598441704289313, 0.3333333333333333703, 0.3079598441704289313, 0.3333333333333333703, 0.3079598441704289313, 0.3333333333333333703, 0.3079598441704289313, 0.3333333333333333703, 0.3079598441704289313, 0.3333333333333333703, 0.3079598441704289313, 0.3333333333333333703, 0.3079598441704289313, 0.3333333333333333703, 0.3079598441704289313, 0.3333333333333333703, 0.3079598441704289313, 0.3333333333333333703, 0.3079598441704289313, 0.3333333333333333703, 0.3251605826665369681, 0.3222526856454325239),
 ( 1.000000000000000000, 0.9238795325112867385, 1.000000000000000000, 0.9238795325112867385, 1.000000000000000000, 0.9238795325112867385, 1.000000000000000000, 0.9238795325112867385, 1.000000000000000000, 0.9238795325112867385, 1.000000000000000000, 0.9238795325112867385, 1.000000000000000000, 0.9238795325112867385, 1.000000000000000000, 0.9238795325112867385, 1.000000000000000000, 0.9238795325112867385, 1.000000000000000000, 0.9238795325112867385, 1.000000000000000000, 0.9238795325112867385, 1.000000000000000000, 0.9238795325112867385, 1.000000000000000000, 0.9238795325112867385, 1.000000000000000000, 0.9238795325112867385, 1.000000000000000000, 0.9238795325112867385, 1.000000000000000000, 0.9238795325112867385, 1.000000000000000000, 0.9238795325112867385, 1.000000000000000000, 0.9238795325112867385, 1.000000000000000000, 0.9238795325112867385, 1.000000000000000000, 0.9238795325112867385, 1.000000000000000000, 0.9238795325112867385, 1.000000000000000000, 0.9238795325112867385, 1.000000000000000000, 0.9238795325112867385, 1.000000000000000000, 0.9238795325112867385, 1.000000000000000000, 0.9238795325112867385, 1.000000000000000000, 0.9238795325112867385, 1.000000000000000000, 0.9238795325112867385, 1.000000000000000000, 0.9238795325112867385, 1.000000000000000000, 0.9238795325112867385, 1.000000000000000000, 0.9238795325112867385, 1.000000000000000000, 0.9238795325112867385, 1.000000000000000000, 0.9238795325112867385, 1.000000000000000000, 0.9238795325112867385, 1.000000000000000000, 0.9238795325112867385, 1.000000000000000000, 0.9238795325112867385, 1.000000000000000000, 0.9238795325112867385, 1.000000000000000000, 0.9238795325112867385, 1.000000000000000000, 0.9238795325112867385, 1.000000000000000000, 0.9238795325112867385, 1.000000000000000000, 0.9238795325112867385, 1.000000000000000000, 0.9238795325112867385, 1.000000000000000000, 0.9238795325112867385, 1.000000000000000000, 0.9238795325112867385, 1.000000000000000000, 0.9238795325112867385, 1.000000000000000000, 0.9238795325112867385, 1.000000000000000000, 0.9238795325112867385, 1.000000000000000000, 0.9754817479996107377, 0.9667580569362973497) ) ) 
 REPRESENTATION_ITEM ( '' )  SURFACE ( )  );
#14832 = ORIENTED_EDGE ( 'NONE', *, *, #2467, .F. ) ;
#14833 = DIRECTION ( 'NONE',  ( 1.000000000000000000, 0.000000000000000000, 0.000000000000000000 ) ) ;
#14834 = ORIENTED_EDGE ( 'NONE', *, *, #6868, .F. ) ;
#14835 = CARTESIAN_POINT ( 'NONE',  ( 2.596731678114175157, -9.937710376390764822, 2.583953520835782225 ) ) ;
#14836 = ORIENTED_EDGE ( 'NONE', *, *, #4800, .F. ) ;
#14837 = CARTESIAN_POINT ( 'NONE',  ( 10.18924542913430820, 0.000000000000000000, 1.000000000000000000 ) ) ;
#14838 = CARTESIAN_POINT ( 'NONE',  ( 13.10624331898488037, 4.052787608736739600, 6.006964772046813117 ) ) ;
#14839 = CARTESIAN_POINT ( 'NONE',  ( 13.50000000000000178, 7.806255641895631925E-15, 1.000000000000000000 ) ) ;
#14840 = CARTESIAN_POINT ( 'NONE',  ( 12.62500016093973620, -20.24999187254239175, 4.532396751752561848 ) ) ;
#14841 = DIRECTION ( 'NONE',  ( 0.000000000000000000, -0.000000000000000000, -1.000000000000000000 ) ) ;
#14842 = CARTESIAN_POINT ( 'NONE',  ( 7.840308582316795949, -22.98484643305508612, 6.020995438708344416 ) ) ;
#14843 = CARTESIAN_POINT ( 'NONE',  ( -12.85087781109329974, -9.593170539812428288, 6.465204579154565145 ) ) ;
#14844 = CARTESIAN_POINT ( 'NONE',  ( -7.559058582316795949, -20.19639159124062999, 5.231925497173373074 ) ) ;
#14845 = FACE_OUTER_BOUND ( 'NONE', #16597, .T. ) ;
#14846 = CARTESIAN_POINT ( 'NONE',  ( 13.42791111847407848, 4.999999999999999112, 1.000000000000000000 ) ) ;
#14847 = EDGE_CURVE ( 'NONE', #15883, #8680, #13260, .T. ) ;
#14848 = CARTESIAN_POINT ( 'NONE',  ( 11.21530858231679595, -23.02099543870833998, 3.136473910504556262 ) ) ;
#14849 = VECTOR ( 'NONE', #7003, 1000.000000000000000 ) ;
#14850 = CARTESIAN_POINT ( 'NONE',  ( -8.597191417683177406, -22.77556120703057729, 5.229004561291656472 ) ) ;
#14851 = ORIENTED_EDGE ( 'NONE', *, *, #19357, .F. ) ;
#14852 = ORIENTED_EDGE ( 'NONE', *, *, #6673, .T. ) ;
#14853 = CARTESIAN_POINT ( 'NONE',  ( 13.87367531042247748, 4.933103176334663331, 5.324010972534209074 ) ) ;
#14854 = CARTESIAN_POINT ( 'NONE',  ( 5.381197846483058989, -14.00000000000000000, 2.000000000000000000 ) ) ;
#14855 = ORIENTED_EDGE ( 'NONE', *, *, #7952, .T. ) ;
#14856 = DIRECTION ( 'NONE',  ( -1.000000000000000000, 0.000000000000000000, 0.000000000000000000 ) ) ;
#14857 = ADVANCED_FACE ( 'NONE', ( #14931 ), #18091, .T. ) ;
#14858 = EDGE_CURVE ( 'NONE', #1213, #9491, #3853, .T. ) ;
#14859 = CARTESIAN_POINT ( 'NONE',  ( -14.49999999999999645, -21.00000000000000355, 4.000000000000000000 ) ) ;
#14860 = CARTESIAN_POINT ( 'NONE',  ( 13.84667963294518778, 4.277765388965502957, 4.000000000000000888 ) ) ;
#14861 = CARTESIAN_POINT ( 'NONE',  ( 13.75871503850933841, -0.8723905552644914962, 5.888179699623941943 ) ) ;
#14862 = CARTESIAN_POINT ( 'NONE',  ( 21.25349085826861995, 11.64110105645932691, 10.00000000000000000 ) ) ;
#14863 = CARTESIAN_POINT ( 'NONE',  ( 1.787053415088318609, -8.367039355952382351, 2.373188808236395886 ) ) ;
#14864 = CARTESIAN_POINT ( 'NONE',  ( 25.04469207716615031, 0.000000000000000000, 0.000000000000000000 ) ) ;
#14865 = VECTOR ( 'NONE', #2986, 1000.000000000000000 ) ;
#14866 = CARTESIAN_POINT ( 'NONE',  ( -12.62966097655984754, -19.26462068372267566, 4.756751955311774083 ) ) ;
#14867 = CARTESIAN_POINT ( 'NONE',  ( 8.590308582316794173, -21.32581373872472952, 1.729004561291657138 ) ) ;
#14868 = DIRECTION ( 'NONE',  ( 0.000000000000000000, 0.000000000000000000, -1.000000000000000000 ) ) ;
#14869 = CARTESIAN_POINT ( 'NONE',  ( 13.10821839766814279, 4.152529082241303904, 5.997503362667785609 ) ) ;
#14870 = CARTESIAN_POINT ( 'NONE',  ( -2.659620708751979645, -10.38426118526329489, 2.698636689302993830 ) ) ;
#14871 = CARTESIAN_POINT ( 'NONE',  ( 6.996558582316795949, -22.05068747287764452, 2.499999999999999112 ) ) ;
#14872 = EDGE_CURVE ( 'NONE', #6318, #10660, #8362, .T. ) ;
#14873 = CARTESIAN_POINT ( 'NONE',  ( 11.50344141768317563, -22.05068747287765873, 5.250000000000000888 ) ) ;
#14874 = CARTESIAN_POINT ( 'NONE',  ( -5.215308582316795949, -23.02099543870833998, 3.136473910504556262 ) ) ;
#14875 = VERTEX_POINT ( 'NONE', #10232 ) ;
#14876 = CARTESIAN_POINT ( 'NONE',  ( 13.11824772738305356, 3.909010232842670796, 6.755569162489314827 ) ) ;
#14877 = CARTESIAN_POINT ( 'NONE',  ( 12.66835678905406049, -17.31048215276408797, 4.799178440007564994 ) ) ;
#14878 = CARTESIAN_POINT ( 'NONE',  ( -12.62499999999990230, -20.15044198641778195, 3.551156945994470071 ) ) ;
#14879 = VERTEX_POINT ( 'NONE', #3755 ) ;
#14880 = ORIENTED_EDGE ( 'NONE', *, *, #14713, .T. ) ;
#14881 = CYLINDRICAL_SURFACE ( 'NONE', #7450, 2.999999999999999112 ) ;
#14882 = DIRECTION ( 'NONE',  ( 1.000000000000000000, 0.000000000000000000, -0.000000000000000000 ) ) ;
#14883 = DIRECTION ( 'NONE',  ( 0.000000000000000000, 0.000000000000000000, -1.000000000000000000 ) ) ;
#14884 = ADVANCED_FACE ( 'NONE', ( #11897 ), #13366, .F. ) ;
#14885 = DIRECTION ( 'NONE',  ( -0.1351665943404306014, -0.9596796555888911229, 0.2464649070825229160 ) ) ;
#14886 = CARTESIAN_POINT ( 'NONE',  ( 1.337453470010121714, -9.864917468222230923, 2.372643865078341019 ) ) ;
#14887 = DIRECTION ( 'NONE',  ( 1.000000000000000000, 0.000000000000000000, 0.000000000000000000 ) ) ;
#14888 = CARTESIAN_POINT ( 'NONE',  ( -5.999999999999999112, -2.500000000000047518, 2.000000000000000000 ) ) ;
#14889 = CARTESIAN_POINT ( 'NONE',  ( 12.62499999999998224, -20.29300445137376485, 3.551156945995087799 ) ) ;
#14890 = DIRECTION ( 'NONE',  ( 1.000000000000000000, 0.000000000000000000, -0.000000000000000000 ) ) ;
#14891 = CARTESIAN_POINT ( 'NONE',  ( -5.590308582316794173, -21.32581373872472597, 1.729004561291657582 ) ) ;
#14892 = CARTESIAN_POINT ( 'NONE',  ( -0.2815691515810352930, -9.114917468222230923, 2.372643865078523984 ) ) ;
#14893 = VERTEX_POINT ( 'NONE', #6999 ) ;
#14894 = AXIS2_PLACEMENT_3D ( 'NONE', #4753, #11139, #19513 ) ;
#14895 = CARTESIAN_POINT ( 'NONE',  ( -13.09560264576187905, 4.265433610975056133, 4.166666666666765551 ) ) ;
#14896 = CARTESIAN_POINT ( 'NONE',  ( -3.500698171653725765, 16.00000000000000000, 1.000000000000000000 ) ) ;
#14897 = ADVANCED_FACE ( 'NONE', ( #2276 ), #19769, .T. ) ;
#14898 = CARTESIAN_POINT ( 'NONE',  ( -7.378441417683176518, -23.74999999999999645, 3.449312527122335492 ) ) ;
#14899 = ORIENTED_EDGE ( 'NONE', *, *, #5885, .F. ) ;
#14900 = EDGE_CURVE ( 'NONE', #11113, #411, #18188, .T. ) ;
#14901 = CARTESIAN_POINT ( 'NONE',  ( 13.37818000216760694, -19.33940989053615311, 4.728953261990445966 ) ) ;
#14902 = DIRECTION ( 'NONE',  ( -0.000000000000000000, -0.000000000000000000, -1.000000000000000000 ) ) ;
#14903 = VERTEX_POINT ( 'NONE', #722 ) ;
#14904 = ORIENTED_EDGE ( 'NONE', *, *, #10792, .T. ) ;
#14905 = CARTESIAN_POINT ( 'NONE',  ( -3.497260319564023057, 4.999999999999999112, 0.000000000000000000 ) ) ;
#14906 = ORIENTED_EDGE ( 'NONE', *, *, #12473, .F. ) ;
#14907 = CARTESIAN_POINT ( 'NONE',  ( -13.37503071710846925, -20.24844878602346299, 4.564052989354591361 ) ) ;
#14908 = ORIENTED_EDGE ( 'NONE', *, *, #11754, .T. ) ;
#14909 = LINE ( 'NONE', #5499, #5319 ) ;
#14910 = EDGE_CURVE ( 'NONE', #1310, #14026, #10339, .T. ) ;
#14911 = PLANE ( 'NONE',  #6993 ) ;
#14912 = DIRECTION ( 'NONE',  ( -1.000000000000000000, 0.000000000000000000, 0.000000000000000000 ) ) ;
#14913 = CARTESIAN_POINT ( 'NONE',  ( 3.211992482548209349, -9.366834950279640637, 2.629956289783360823 ) ) ;
#14914 = CARTESIAN_POINT ( 'NONE',  ( 0.000000000000000000, 10.00000000000000000, 1.000000000000000000 ) ) ;
#14915 = CARTESIAN_POINT ( 'NONE',  ( 12.65986935584910000, -19.23909752961862907, 6.257782094979345899 ) ) ;
#14916 = LINE ( 'NONE', #2260, #9625 ) ;
#14917 = CARTESIAN_POINT ( 'NONE',  ( 9.159691417683179182, -22.67418626127524917, 1.729004561291651809 ) ) ;
#14918 = FACE_OUTER_BOUND ( 'NONE', #13974, .T. ) ;
#14919 = CARTESIAN_POINT ( 'NONE',  ( -4.753441417683176518, -21.94931252712233061, 2.499999999999999112 ) ) ;
#14920 = CARTESIAN_POINT ( 'NONE',  ( -6.715308582316796837, -24.52099543870834708, 2.515153566944913432 ) ) ;
#14921 = ORIENTED_EDGE ( 'NONE', *, *, #9122, .F. ) ;
#14922 = CARTESIAN_POINT ( 'NONE',  ( 12.64931222250080545, -19.02223276370786209, 5.512399842915133519 ) ) ;
#14923 = CARTESIAN_POINT ( 'NONE',  ( -13.15498530132288479, 5.764257716805535559, 4.916666666666649199 ) ) ;
#14924 = EDGE_LOOP ( 'NONE', ( #11283, #9462, #5417, #6860 ) ) ;
#14925 = DIRECTION ( 'NONE',  ( 3.469446951953491127E-15, 1.000000000000000000, -0.000000000000000000 ) ) ;
#14926 = DIRECTION ( 'NONE',  ( 1.000000000000000000, 0.000000000000000000, -0.000000000000000000 ) ) ;
#14927 = ORIENTED_EDGE ( 'NONE', *, *, #15655, .T. ) ;
#14928 = ORIENTED_EDGE ( 'NONE', *, *, #8519, .F. ) ;
#14929 = CARTESIAN_POINT ( 'NONE',  ( 13.28039013372821131, -20.00084031961838704, 3.461764366045932295 ) ) ;
#14930 = ORIENTED_EDGE ( 'NONE', *, *, #6786, .F. ) ;
#14931 = FACE_OUTER_BOUND ( 'NONE', #10639, .T. ) ;
#14932 = EDGE_CURVE ( 'NONE', #1434, #5711, #5629, .T. ) ;
#14933 = LINE ( 'NONE', #16306, #924 ) ;
#14934 = CARTESIAN_POINT ( 'NONE',  ( -1.720709671993384093, -9.114925383610804843, 1.622645897908254753 ) ) ;
#14935 = PLANE ( 'NONE',  #11025 ) ;
#14936 = DIRECTION ( 'NONE',  ( 0.000000000000000000, 0.000000000000000000, 1.000000000000000000 ) ) ;
#14937 = VECTOR ( 'NONE', #16023, 1000.000000000000000 ) ;
#14938 = CARTESIAN_POINT ( 'NONE',  ( 18.44064177244175440, 11.64110105645932691, 10.00000000000000000 ) ) ;
#14939 = CARTESIAN_POINT ( 'NONE',  ( -14.56494360078803396, 11.64110105645932691, 0.000000000000000000 ) ) ;
#14940 = VECTOR ( 'NONE', #11183, 1000.000000000000000 ) ;
#14941 = CARTESIAN_POINT ( 'NONE',  ( 8.965308582316795949, -19.47900456129164937, 4.484846433055089676 ) ) ;
#14942 = CARTESIAN_POINT ( 'NONE',  ( -12.70700162295422864, -16.85891804079483691, 6.308954579156044851 ) ) ;
#14943 = CARTESIAN_POINT ( 'NONE',  ( -7.659691417683177406, -22.98484643305507191, 0.9790045612916508100 ) ) ;
#14944 = CARTESIAN_POINT ( 'NONE',  ( 0.000000000000000000, 10.00000000000000000, 1.000000000000000000 ) ) ;
#14945 = LINE ( 'NONE', #321, #19774 ) ;
#14946 = CARTESIAN_POINT ( 'NONE',  ( 12.15280858231679950, -21.53509896474924901, 4.479004561291659137 ) ) ;
#14947 = CARTESIAN_POINT ( 'NONE',  ( -3.974842109207561425, -21.82955800590261930, 5.256404853634145447 ) ) ;
#14948 = ORIENTED_EDGE ( 'NONE', *, *, #11165, .T. ) ;
#14949 = ORIENTED_EDGE ( 'NONE', *, *, #9673, .F. ) ;
#14950 = CARTESIAN_POINT ( 'NONE',  ( 13.87470602645761986, 4.985154336109792972, 4.916666666666650087 ) ) ;
#14951 = DIRECTION ( 'NONE',  ( 1.000000000000000000, 0.000000000000000000, -0.000000000000000000 ) ) ;
#14952 =( LENGTH_UNIT ( ) NAMED_UNIT ( * ) SI_UNIT ( .MILLI., .METRE. ) );
#14953 = ORIENTED_EDGE ( 'NONE', *, *, #16436, .T. ) ;
#14954 = DIRECTION ( 'NONE',  ( 1.000000000000000000, 0.000000000000000000, 0.000000000000000000 ) ) ;
#14955 = CARTESIAN_POINT ( 'NONE',  ( 5.999999999999999112, -7.500000000000047073, 8.999999999999998224 ) ) ;
#14956 = VECTOR ( 'NONE', #17770, 1000.000000000000000 ) ;
#14957 = FACE_OUTER_BOUND ( 'NONE', #6346, .T. ) ;
#14958 = CARTESIAN_POINT ( 'NONE',  ( 13.85980676119184629, 4.232741440188380722, 5.965367510457697975 ) ) ;
#14959 = PLANE ( 'NONE',  #15542 ) ;
#14960 = CARTESIAN_POINT ( 'NONE',  ( 3.270401025279431995, -9.547343748290430199, 2.676314555138040063 ) ) ;
#14961 = ADVANCED_FACE ( 'NONE', ( #16305 ), #9085, .T. ) ;
#14962 = CARTESIAN_POINT ( 'NONE',  ( -26.94203811574920593, 11.64110105645932691, 0.000000000000000000 ) ) ;
#14963 = CARTESIAN_POINT ( 'NONE',  ( -12.62499999999998401, -19.49999999999998934, 2.439580858552613751 ) ) ;
#14964 = CARTESIAN_POINT ( 'NONE',  ( 5.590308582316794173, -21.32581373872472952, 1.729004561291657138 ) ) ;
#14965 = CARTESIAN_POINT ( 'NONE',  ( 1.811130159782011528, 0.000000000000000000, 0.000000000000000000 ) ) ;
#14966 = CARTESIAN_POINT ( 'NONE',  ( 12.66369984131459070, -18.29565801360988075, 5.528024842915327142 ) ) ;
#14967 = VECTOR ( 'NONE', #8860, 1000.000000000000000 ) ;
#14968 = CARTESIAN_POINT ( 'NONE',  ( 0.000000000000000000, -9.864917468222230923, 2.372643865078341019 ) ) ;
#14969 = EDGE_CURVE ( 'NONE', #17844, #2663, #10449, .T. ) ;
#14970 = CARTESIAN_POINT ( 'NONE',  ( 11.49655858231679595, -22.05068747287764452, 2.499999999999999112 ) ) ;
#14971 = EDGE_CURVE ( 'NONE', #6994, #18278, #9181, .T. ) ;
#14972 = CARTESIAN_POINT ( 'NONE',  ( 11.69094141768317563, -23.27327832286946219, 4.701595411283453707 ) ) ;
#14973 = CARTESIAN_POINT ( 'NONE',  ( -8.027808582316792396, -23.72900456129165647, 4.275561207030568411 ) ) ;
#14974 = ORIENTED_EDGE ( 'NONE', *, *, #20641, .F. ) ;
#14975 = CARTESIAN_POINT ( 'NONE',  ( 12.75496035233418013, -14.43700220713569138, 6.361037912489419632 ) ) ;
#14976 = AXIS2_PLACEMENT_3D ( 'NONE', #18912, #4570, #15757 ) ;
#14977 = CARTESIAN_POINT ( 'NONE',  ( 13.09300823383486900, 4.134415808666423331, 5.226944302881396887 ) ) ;
#14978 = DIRECTION ( 'NONE',  ( 1.000000000000000000, 0.000000000000000000, 0.000000000000000000 ) ) ;
#14979 = ORIENTED_EDGE ( 'NONE', *, *, #718, .T. ) ;
#14980 = ORIENTED_EDGE ( 'NONE', *, *, #5301, .F. ) ;
#14981 = CARTESIAN_POINT ( 'NONE',  ( -15.49999999999999822, -20.99999999999999645, 1.000000000000000000 ) ) ;
#14982 = AXIS2_PLACEMENT_3D ( 'NONE', #16257, #5477, #11850 ) ;
#14983 = CARTESIAN_POINT ( 'NONE',  ( 0.000000000000000000, 11.64110105645932691, 10.00000000000000000 ) ) ;
#14984 = VECTOR ( 'NONE', #6847, 1000.000000000000000 ) ;
#14985 = LINE ( 'NONE', #1924, #9316 ) ;
#14986 = ADVANCED_FACE ( 'NONE', ( #7305 ), #13980, .T. ) ;
#14987 = LINE ( 'NONE', #2031, #1984 ) ;
#14988 = CARTESIAN_POINT ( 'NONE',  ( 0.9854920305337621089, -9.114917468222230923, 2.372643865078341019 ) ) ;
#14989 = CARTESIAN_POINT ( 'NONE',  ( -24.12918902992234393, 11.64110105645932691, 10.00000000000000000 ) ) ;
#14990 = LINE ( 'NONE', #8518, #18081 ) ;
#14991 = CARTESIAN_POINT ( 'NONE',  ( 12.71341536712609965, -20.49194379261451715, 3.539064175304416082 ) ) ;
#14992 = CARTESIAN_POINT ( 'NONE',  ( 0.000000000000000000, 4.999999999999999112, 1.000000000000000000 ) ) ;
#14993 = CARTESIAN_POINT ( 'NONE',  ( -6.902808582316793284, -22.77556120703056308, 1.770995438708339975 ) ) ;
#14994 = CARTESIAN_POINT ( 'NONE',  ( -3.521144778809589315, -10.09312707791070096, 2.066482617302010105 ) ) ;
#14995 = VECTOR ( 'NONE', #15095, 1000.000000000000000 ) ;
#14996 = VERTEX_POINT ( 'NONE', #12520 ) ;
#14997 = CARTESIAN_POINT ( 'NONE',  ( -13.37732542738919328, -19.38256591684242025, 4.710253041318374301 ) ) ;
#14998 = CARTESIAN_POINT ( 'NONE',  ( -5.121558582316794173, -23.74999999999999645, 3.550687472877651629 ) ) ;
#14999 = CARTESIAN_POINT ( 'NONE',  ( -11.50344141768317741, -22.05068747287766229, 4.499999999999999112 ) ) ;
#15000 = VECTOR ( 'NONE', #1868, 1000.000000000000000 ) ;
#15001 = ORIENTED_EDGE ( 'NONE', *, *, #2817, .T. ) ;
#15002 = CARTESIAN_POINT ( 'NONE',  ( 13.39359219590679295, -19.31109410670777038, 5.491647114909025795 ) ) ;
#15003 = LINE ( 'NONE', #12178, #19416 ) ;
#15004 = ORIENTED_EDGE ( 'NONE', *, *, #339, .T. ) ;
#15005 = EDGE_CURVE ( 'NONE', #999, #4851, #10648, .T. ) ;
#15006 = ORIENTED_EDGE ( 'NONE', *, *, #17922, .F. ) ;
#15007 = DIRECTION ( 'NONE',  ( 0.000000000000000000, 0.000000000000000000, 1.000000000000000000 ) ) ;
#15008 = VERTEX_POINT ( 'NONE', #7418 ) ;
#15009 = CARTESIAN_POINT ( 'NONE',  ( -13.37597619100657198, -20.20070235416671167, 4.815535977982682070 ) ) ;
#15010 = ORIENTED_EDGE ( 'NONE', *, *, #5398, .T. ) ;
#15011 = LINE ( 'NONE', #17951, #973 ) ;
#15012 = LINE ( 'NONE', #16577, #5990 ) ;
#15013 = EDGE_CURVE ( 'NONE', #18054, #18680, #5939, .T. ) ;
#15014 = VECTOR ( 'NONE', #17823, 1000.000000000000000 ) ;
#15015 = EDGE_CURVE ( 'NONE', #11469, #19731, #7517, .T. ) ;
#15016 = CARTESIAN_POINT ( 'NONE',  ( -13.87500000000000000, 5.000000000000049738, 4.000000000000000888 ) ) ;
#15017 = CARTESIAN_POINT ( 'NONE',  ( 3.594802210173583035, -11.77224174634763898, 3.247712807842289884 ) ) ;
#15018 = CARTESIAN_POINT ( 'NONE',  ( -7.277808582316795061, -20.27099543870833642, 2.724438792969431589 ) ) ;
#15019 = VECTOR ( 'NONE', #12452, 1000.000000000000000 ) ;
#15020 = CARTESIAN_POINT ( 'NONE',  ( 13.90439735423465351, 5.734566389025032684, 3.333333333332063386 ) ) ;
#15021 = PLANE ( 'NONE',  #16636 ) ;
#15022 = CARTESIAN_POINT ( 'NONE',  ( 10.65969141768317741, -22.36352608949543352, 2.479004561291652031 ) ) ;
#15023 = CARTESIAN_POINT ( 'NONE',  ( -12.62888984277510218, -20.05356293986039873, 5.111704976569332537 ) ) ;
#15024 = CARTESIAN_POINT ( 'NONE',  ( -4.659691417683177406, -22.36352608949543352, 2.479004561291652031 ) ) ;
#15025 = CARTESIAN_POINT ( 'NONE',  ( -8.496558582316795949, -22.05068747287764452, 0.9999999999999978906 ) ) ;
#15026 = ORIENTED_EDGE ( 'NONE', *, *, #17663, .F. ) ;
#15027 = CARTESIAN_POINT ( 'NONE',  ( 13.12529397354238192, 5.014845663890295846, 4.791666666666685614 ) ) ;
#15028 = CARTESIAN_POINT ( 'NONE',  ( -12.69247507894198712, -16.84250851341299082, 5.559274842915185033 ) ) ;
#15029 = ORIENTED_EDGE ( 'NONE', *, *, #18172, .T. ) ;
#15030 = CARTESIAN_POINT ( 'NONE',  ( 3.499999999999998668, -19.50000000000000000, 4.000000000000000000 ) ) ;
#15031 = CYLINDRICAL_SURFACE ( 'NONE', #14001, 0.5000000000000000000 ) ;
#15032 =( GEOMETRIC_REPRESENTATION_CONTEXT ( 3 ) GLOBAL_UNCERTAINTY_ASSIGNED_CONTEXT ( ( #15704 ) ) GLOBAL_UNIT_ASSIGNED_CONTEXT ( ( #11919, #1056, #11820 ) ) REPRESENTATION_CONTEXT ( 'NONE', 'WORKASPACE' ) );
#15033 = EDGE_LOOP ( 'NONE', ( #18961, #10151, #6098, #10823 ) ) ;
#15034 = VERTEX_POINT ( 'NONE', #10757 ) ;
#15035 = AXIS2_PLACEMENT_3D ( 'NONE', #60, #14688, #369 ) ;
#15036 = CARTESIAN_POINT ( 'NONE',  ( -14.00000000000000355, -9.599706735548742312E-18, 0.5896324317178637253 ) ) ;
#15037 = ORIENTED_EDGE ( 'NONE', *, *, #2402, .T. ) ;
#15038 = DIRECTION ( 'NONE',  ( 1.000000000000000000, 0.000000000000000000, 0.000000000000000000 ) ) ;
#15039 = CARTESIAN_POINT ( 'NONE',  ( 13.10372118337080849, 3.925419760224517329, 6.005889426248455010 ) ) ;
#15040 = CARTESIAN_POINT ( 'NONE',  ( -1.754777266914451461, -9.116337928146160507, 1.623008667563337726 ) ) ;
#15041 = CARTESIAN_POINT ( 'NONE',  ( -27.94203811574921659, 9.999999999999998224, 1.000000000000000000 ) ) ;
#15042 = CARTESIAN_POINT ( 'NONE',  ( -3.497260319564023057, 4.999999999999999112, 1.000000000000000000 ) ) ;
#15043 = CARTESIAN_POINT ( 'NONE',  ( 13.12463908936614132, 4.981774012991869505, 5.264611377988129171 ) ) ;
#15044 = CARTESIAN_POINT ( 'NONE',  ( -17.11324865405191176, -11.00000000000000000, 1.000000000000000000 ) ) ;
#15045 = CARTESIAN_POINT ( 'NONE',  ( 6.902808582316795949, -23.08622137881038938, 1.020995438708339309 ) ) ;
#15046 = CARTESIAN_POINT ( 'NONE',  ( -13.12529397354238192, 5.014845663890295846, 4.666666666666619889 ) ) ;
#15047 = VECTOR ( 'NONE', #16569, 1000.000000000000000 ) ;
#15048 = CARTESIAN_POINT ( 'NONE',  ( -7.847191417683175629, -20.91377862118959285, 1.020995438708345082 ) ) ;
#15049 = VECTOR ( 'NONE', #11225, 1000.000000000000000 ) ;
#15050 = VECTOR ( 'NONE', #3266, 1000.000000000000000 ) ;
#15051 = ORIENTED_EDGE ( 'NONE', *, *, #4304, .T. ) ;
#15052 = FACE_OUTER_BOUND ( 'NONE', #6956, .T. ) ;
#15053 = DIRECTION ( 'NONE',  ( 0.000000000000000000, 0.000000000000000000, 1.000000000000000000 ) ) ;
#15054 = CARTESIAN_POINT ( 'NONE',  ( -13.40621837757088564, -18.67347193267085714, 5.505367199623145247 ) ) ;
#15055 = ADVANCED_FACE ( 'NONE', ( #7613 ), #15454, .T. ) ;
#15056 = CARTESIAN_POINT ( 'NONE',  ( 9.340308582316795949, -22.36352608949544418, 4.520995438708343528 ) ) ;
#15057 = CARTESIAN_POINT ( 'NONE',  ( 5.381197846483058989, -6.000000000000000000, 1.000000000000000000 ) ) ;
#15058 = EDGE_LOOP ( 'NONE', ( #151, #15528, #15062, #9253 ) ) ;
#15059 = ORIENTED_EDGE ( 'NONE', *, *, #13617, .F. ) ;
#15060 = CARTESIAN_POINT ( 'NONE',  ( 13.85528666703740619, 4.004476685417483139, 5.993048563355776182 ) ) ;
#15061 = FACE_OUTER_BOUND ( 'NONE', #10546, .T. ) ;
#15062 = ORIENTED_EDGE ( 'NONE', *, *, #5535, .T. ) ;
#15063 = LINE ( 'NONE', #16430, #4450 ) ;
#15064 = CARTESIAN_POINT ( 'NONE',  ( 13.49999999999998401, -18.49999999999999645, 4.000000000000000000 ) ) ;
#15065 = CARTESIAN_POINT ( 'NONE',  ( 0.000000000000000000, 4.999999999999999112, 0.000000000000000000 ) ) ;
#15066 = VECTOR ( 'NONE', #15715, 1000.000000000000000 ) ;
#15067 = CARTESIAN_POINT ( 'NONE',  ( 13.39296152110871851, -19.34294318400601753, 5.489418334493660012 ) ) ;
#15068 = PRODUCT_RELATED_PRODUCT_CATEGORY ( 'part', '', ( #1835 ) ) ;
#15069 = DIRECTION ( 'NONE',  ( 1.000000000000000000, 0.000000000000000000, 0.000000000000000000 ) ) ;
#15070 = CARTESIAN_POINT ( 'NONE',  ( 3.451187703687236041, -10.75258211228477734, 2.985843844067104680 ) ) ;
#15071 = CARTESIAN_POINT ( 'NONE',  ( -16.62779268661489951, 10.00000000000000000, 0.000000000000000000 ) ) ;
#15072 = CARTESIAN_POINT ( 'NONE',  ( -12.63036675113625407, -19.22897906761645004, 4.757923088130392664 ) ) ;
#15073 = CARTESIAN_POINT ( 'NONE',  ( 30.00000000000000000, 3.000000000000000000, 1.000000000000000000 ) ) ;
#15074 = CARTESIAN_POINT ( 'NONE',  ( 12.99655858231679417, -22.05068747287764452, 1.749999999999998446 ) ) ;
#15075 = CARTESIAN_POINT ( 'NONE',  ( 13.11017182064853159, 4.251176942750957366, 5.979809059808775196 ) ) ;
#15076 = CARTESIAN_POINT ( 'NONE',  ( -1.513434189748285696, -9.114917468222230923, 2.372643865078341019 ) ) ;
#15077 = CARTESIAN_POINT ( 'NONE',  ( 8.871558582316795949, -20.99999999999999645, 3.449312527122348371 ) ) ;
#15078 = AXIS2_PLACEMENT_3D ( 'NONE', #11904, #13371, #12402 ) ;
#15079 = CARTESIAN_POINT ( 'NONE',  ( 6.628441417683176518, -20.24999999999999289, 3.550687472877664952 ) ) ;
#15080 = CARTESIAN_POINT ( 'NONE',  ( -11.68405858231679417, -20.79840458871652942, 2.226721677130544030 ) ) ;
#15081 = VERTEX_POINT ( 'NONE', #9281 ) ;
#15082 = CARTESIAN_POINT ( 'NONE',  ( 12.65679946139692902, -19.39412719945235253, 6.251687395662565372 ) ) ;
#15083 = CARTESIAN_POINT ( 'NONE',  ( 12.62525331949183105, -19.48720736566255951, 4.581880915780448760 ) ) ;
#15084 = CARTESIAN_POINT ( 'NONE',  ( -11.24178095869206828, 0.000000000000000000, 1.000000000000000000 ) ) ;
#15085 = VERTEX_POINT ( 'NONE', #16819 ) ;
#15086 = ADVANCED_FACE ( 'NONE', ( #13779 ), #4480, .T. ) ;
#15087 = APPLICATION_CONTEXT ( 'automotive_design' ) ;
#15088 = VERTEX_POINT ( 'NONE', #5742 ) ;
#15089 = DIRECTION ( 'NONE',  ( 0.000000000000000000, 0.000000000000000000, 1.000000000000000000 ) ) ;
#15090 = DIRECTION ( 'NONE',  ( 0.000000000000000000, 1.000000000000000000, -0.000000000000000000 ) ) ;
#15091 = EDGE_CURVE ( 'NONE', #15857, #8796, #16324, .T. ) ;
#15092 = EDGE_CURVE ( 'NONE', #5162, #12182, #15659, .T. ) ;
#15093 = CARTESIAN_POINT ( 'NONE',  ( 5.381197846483058989, -14.00000000000000000, 2.000000000000000000 ) ) ;
#15094 = VECTOR ( 'NONE', #7993, 1000.000000000000000 ) ;
#15095 = DIRECTION ( 'NONE',  ( 0.000000000000000000, -1.000000000000000000, 0.000000000000000000 ) ) ;
#15096 = CARTESIAN_POINT ( 'NONE',  ( 1.742625132518061504, -9.872369070458363538, 2.374557585393312298 ) ) ;
#15097 = CARTESIAN_POINT ( 'NONE',  ( 0.000000000000000000, 0.000000000000000000, 1.000000000000000000 ) ) ;
#15098 = CARTESIAN_POINT ( 'NONE',  ( -13.87500000000000178, 5.000000000000047962, 2.000000000000000000 ) ) ;
#15099 = VECTOR ( 'NONE', #12674, 1000.000000000000000 ) ;
#15100 = CARTESIAN_POINT ( 'NONE',  ( 13.33061827858665893, -20.43393009137478344, 3.455122606006641561 ) ) ;
#15101 = LINE ( 'NONE', #18040, #4974 ) ;
#15102 = CARTESIAN_POINT ( 'NONE',  ( -5.402808582316794173, -22.77556120703056308, 1.770995438708339975 ) ) ;
#15103 = CARTESIAN_POINT ( 'NONE',  ( -1.126276606324276619, -8.364917468222230923, 2.372643865078341019 ) ) ;
#15104 = ORIENTED_EDGE ( 'NONE', *, *, #5687, .F. ) ;
#15105 = CARTESIAN_POINT ( 'NONE',  ( -13.09560264576187905, 4.265433610975056133, 4.916666666666649199 ) ) ;
#15106 = VECTOR ( 'NONE', #18112, 1000.000000000000114 ) ;
#15107 = CARTESIAN_POINT ( 'NONE',  ( -9.902808582316794173, -22.77556120703056308, 1.770995438708339975 ) ) ;
#15108 = CARTESIAN_POINT ( 'NONE',  ( 7.652808582316796837, -20.91377862118960351, 5.979004561291660913 ) ) ;
#15109 = CARTESIAN_POINT ( 'NONE',  ( -7.190941417683177406, -22.74294823697955081, 4.171265325393542334 ) ) ;
#15110 = ORIENTED_EDGE ( 'NONE', *, *, #15196, .T. ) ;
#15111 = CARTESIAN_POINT ( 'NONE',  ( 13.37741471237955260, -20.12805702483293757, 4.993653275319895890 ) ) ;
#15112 = CARTESIAN_POINT ( 'NONE',  ( -2.693754455098655409, -10.14181605509423711, 1.874202551270839123 ) ) ;
#15113 = VERTEX_POINT ( 'NONE', #17021 ) ;
#15114 = ORIENTED_EDGE ( 'NONE', *, *, #7540, .T. ) ;
#15115 = VECTOR ( 'NONE', #20326, 1000.000000000000000 ) ;
#15116 = CARTESIAN_POINT ( 'NONE',  ( -3.499999999999997780, -24.49999999999999289, 1.000000000000000000 ) ) ;
#15117 = EDGE_CURVE ( 'NONE', #12575, #14721, #13879, .T. ) ;
#15118 = ORIENTED_EDGE ( 'NONE', *, *, #55, .F. ) ;
#15119 = CARTESIAN_POINT ( 'NONE',  ( -13.37499999999998579, -20.24999999999999289, 3.482947684955674639 ) ) ;
#15120 = EDGE_CURVE ( 'NONE', #5545, #20631, #6980, .T. ) ;
#15121 = ADVANCED_FACE ( 'NONE', ( #17127 ), #2907, .F. ) ;
#15122 = ORIENTED_EDGE ( 'NONE', *, *, #18999, .F. ) ;
#15123 = CARTESIAN_POINT ( 'NONE',  ( -5.433390479346035029, 9.000000000000001776, 1.000000000000000000 ) ) ;
#15124 = CARTESIAN_POINT ( 'NONE',  ( 5.999999999999999112, -2.500000000000047518, 8.999999999999998224 ) ) ;
#15125 = DIRECTION ( 'NONE',  ( 1.000000000000000000, 0.000000000000000000, 0.000000000000000000 ) ) ;
#15126 = CARTESIAN_POINT ( 'NONE',  ( 1.787053415088318609, -8.367039355952382351, 2.373188808236395886 ) ) ;
#15127 = CARTESIAN_POINT ( 'NONE',  ( -8.121558582316792396, -23.74999999999999645, 3.550687472877651629 ) ) ;
#15128 = EDGE_CURVE ( 'NONE', #13259, #12874, #6052, .T. ) ;
#15129 = VECTOR ( 'NONE', #6076, 1000.000000000000000 ) ;
#15130 = CARTESIAN_POINT ( 'NONE',  ( 13.90326467458556969, 5.677366066573198644, 5.457668599364335904 ) ) ;
#15131 = CARTESIAN_POINT ( 'NONE',  ( -14.99999999999999645, -30.00000000000000711, 0.000000000000000000 ) ) ;
#15132 = CARTESIAN_POINT ( 'NONE',  ( 5.034691417683178294, -20.22900456129164581, 2.825813738724747726 ) ) ;
#15133 = CARTESIAN_POINT ( 'NONE',  ( -24.79469207716615031, 0.000000000000000000, 0.000000000000000000 ) ) ;
#15134 = CARTESIAN_POINT ( 'NONE',  ( -4.565941417683176518, -22.67126532539353789, 2.757051763020445634 ) ) ;
#15135 = CARTESIAN_POINT ( 'NONE',  ( -5.027808582316795949, -24.47900456129166358, 4.586221378810390270 ) ) ;
#15136 = ORIENTED_EDGE ( 'NONE', *, *, #12931, .F. ) ;
#15137 = CARTESIAN_POINT ( 'NONE',  ( 12.64197948789552051, -18.64253586127677309, 4.770532606674187548 ) ) ;
#15138 = CARTESIAN_POINT ( 'NONE',  ( -13.12529397354238192, 5.014845663890295846, 4.583333333333296622 ) ) ;
#15139 = ORIENTED_EDGE ( 'NONE', *, *, #3761, .T. ) ;
#15140 = DIRECTION ( 'NONE',  ( 1.000000000000000000, 0.000000000000000000, 0.000000000000000000 ) ) ;
#15141 = EDGE_CURVE ( 'NONE', #6665, #19457, #20495, .T. ) ;
#15142 = CARTESIAN_POINT ( 'NONE',  ( 7.500000000000002665, -9.999999999999991118, 2.000000000000000000 ) ) ;
#15143 = ORIENTED_EDGE ( 'NONE', *, *, #19705, .F. ) ;
#15144 = ITEM_DEFINED_TRANSFORMATION ( 'NONE', 'NONE', #17728,  #18039 ) ;
#15145 = ORIENTED_EDGE ( 'NONE', *, *, #608, .F. ) ;
#15146 = ORIENTED_EDGE ( 'NONE', *, *, #3524, .F. ) ;
#15147 = DIRECTION ( 'NONE',  ( -0.000000000000000000, -0.000000000000000000, -1.000000000000000000 ) ) ;
#15148 = FACE_OUTER_BOUND ( 'NONE', #18184, .T. ) ;
#15149 = CARTESIAN_POINT ( 'NONE',  ( -2.722060606927515725, -8.660968749821154944, 1.698675748411476283 ) ) ;
#15150 = LINE ( 'NONE', #2390, #668 ) ;
#15151 = CARTESIAN_POINT ( 'NONE',  ( 15.50000000000000178, -23.00000000000000711, 4.000000000000000000 ) ) ;
#15152 = EDGE_CURVE ( 'NONE', #12662, #3823, #15860, .T. ) ;
#15153 = DIRECTION ( 'NONE',  ( 1.000000000000000000, 0.000000000000000000, 0.000000000000000000 ) ) ;
#15154 = CARTESIAN_POINT ( 'NONE',  ( 10.47219141768317741, -24.47900456129165292, 2.413778621189595963 ) ) ;
#15155 = CARTESIAN_POINT ( 'NONE',  ( -13.12424783836753228, 4.962015837561366993, 5.328858059679200565 ) ) ;
#15156 = CARTESIAN_POINT ( 'NONE',  ( -4.003441417683175629, -22.05068747287766229, 6.000000000000001776 ) ) ;
#15157 = EDGE_LOOP ( 'NONE', ( #8022, #11968, #13612, #5741 ) ) ;
#15158 = CARTESIAN_POINT ( 'NONE',  ( 12.90280858231679773, -22.77556120703056308, 1.770995438708339975 ) ) ;
#15159 = LINE ( 'NONE', #13580, #11749 ) ;
#15160 = CARTESIAN_POINT ( 'NONE',  ( -13.86436316834274329, 3.712840001305938831, 6.736817769197426031 ) ) ;
#15161 = CARTESIAN_POINT ( 'NONE',  ( 13.27780858231679595, -20.27099543870833642, 2.724438792969431589 ) ) ;
#15162 = EDGE_CURVE ( 'NONE', #5259, #8157, #8136, .T. ) ;
#15163 = FACE_OUTER_BOUND ( 'NONE', #14567, .T. ) ;
#15164 = ORIENTED_EDGE ( 'NONE', *, *, #5701, .F. ) ;
#15165 = EDGE_LOOP ( 'NONE', ( #11162, #11916, #20587, #16144 ) ) ;
#15166 = CARTESIAN_POINT ( 'NONE',  ( 13.87470602645761986, 4.985154336109792972, 4.333333333333382775 ) ) ;
#15167 = FACE_OUTER_BOUND ( 'NONE', #7265, .T. ) ;
#15168 = PRESENTATION_STYLE_ASSIGNMENT (( #8800 ) ) ;
#15169 = VERTEX_POINT ( 'NONE', #19130 ) ;
#15170 = DIRECTION ( 'NONE',  ( 1.000000000000000000, 0.000000000000000000, 0.000000000000000000 ) ) ;
#15171 = LINE ( 'NONE', #10056, #9028 ) ;
#15172 = LINE ( 'NONE', #18215, #1309 ) ;
#15173 = CARTESIAN_POINT ( 'NONE',  ( 13.87470602645761986, 4.985154336109792972, 4.833333333333344584 ) ) ;
#15174 = CARTESIAN_POINT ( 'NONE',  ( 23.60856191738414012, 4.999999999999999112, 0.000000000000000000 ) ) ;
#15175 = CARTESIAN_POINT ( 'NONE',  ( 1.655860418491166941, -9.114909740826840689, 2.372641880528837621 ) ) ;
#15176 = EDGE_CURVE ( 'NONE', #2288, #9910, #19015, .T. ) ;
#15177 = DIRECTION ( 'NONE',  ( -0.000000000000000000, 0.000000000000000000, -1.000000000000000000 ) ) ;
#15178 = CARTESIAN_POINT ( 'NONE',  ( -12.64197948789552051, -18.64253586127677309, 4.770532606674187548 ) ) ;
#15179 = LINE ( 'NONE', #1244, #15968 ) ;
#15180 = FACE_OUTER_BOUND ( 'NONE', #10723, .T. ) ;
#15181 = CARTESIAN_POINT ( 'NONE',  ( -13.87470602645761986, 4.985154336109792972, 4.166666666666765551 ) ) ;
#15182 = CARTESIAN_POINT ( 'NONE',  ( 0.000000000000000000, 16.00000000000000000, 1.000000000000000000 ) ) ;
#15183 = CARTESIAN_POINT ( 'NONE',  ( 11.30905858231679417, -23.27327832286945153, 2.298404588716537411 ) ) ;
#15184 = CARTESIAN_POINT ( 'NONE',  ( 9.534691417683177406, -20.97900456129164581, 3.136473910504570917 ) ) ;
#15185 = CARTESIAN_POINT ( 'NONE',  ( -9.715308582316794173, -23.77099543870833998, 2.825813738724734847 ) ) ;
#15186 = ORIENTED_EDGE ( 'NONE', *, *, #6414, .T. ) ;
#15187 = CARTESIAN_POINT ( 'NONE',  ( 12.66863463945108137, -18.79645070772368953, 6.267287912489321045 ) ) ;
#15188 = CARTESIAN_POINT ( 'NONE',  ( 12.62562661273123332, -19.46835605706984040, 4.628101975944573176 ) ) ;
#15189 = LINE ( 'NONE', #15497, #335 ) ;
#15190 = ORIENTED_EDGE ( 'NONE', *, *, #6829, .F. ) ;
#15191 = ORIENTED_EDGE ( 'NONE', *, *, #14910, .T. ) ;
#15192 = CARTESIAN_POINT ( 'NONE',  ( 25.54469207716615031, 4.999999999999999112, 1.000000000000000000 ) ) ;
#15193 = FACE_OUTER_BOUND ( 'NONE', #12204, .T. ) ;
#15194 = AXIS2_PLACEMENT_3D ( 'NONE', #12034, #18428, #16846 ) ;
#15195 = CARTESIAN_POINT ( 'NONE',  ( -13.49999999999998401, -19.49999999999999645, 4.000000000000000000 ) ) ;
#15196 = EDGE_CURVE ( 'NONE', #13563, #18369, #19127, .T. ) ;
#15197 = CARTESIAN_POINT ( 'NONE',  ( 27.00000000000000000, 3.000000000000000000, 0.000000000000000000 ) ) ;
#15198 = CARTESIAN_POINT ( 'NONE',  ( 1.513434189748285696, -9.114917468222230923, 2.372643865078341019 ) ) ;
#15199 = CARTESIAN_POINT ( 'NONE',  ( -15.87779268661489773, 10.00000000000000000, 1.000000000000000000 ) ) ;
#15200 = LINE ( 'NONE', #8929, #1714 ) ;
#15201 = EDGE_CURVE ( 'NONE', #17667, #7935, #14909, .T. ) ;
#15202 = CARTESIAN_POINT ( 'NONE',  ( 10.38119784648305810, -14.00000000000000000, 2.000000000000000000 ) ) ;
#15203 = CARTESIAN_POINT ( 'NONE',  ( -9.996558582316795949, -22.05068747287764452, 0.9999999999999978906 ) ) ;
#15204 = CARTESIAN_POINT ( 'NONE',  ( -1.619022621591187150, -9.114917468222230923, 1.622643865078341463 ) ) ;
#15205 = ORIENTED_EDGE ( 'NONE', *, *, #17827, .T. ) ;
#15206 = CARTESIAN_POINT ( 'NONE',  ( -13.09559422631463654, 4.265008428887424152, 5.017082219073495608 ) ) ;
#15207 = CARTESIAN_POINT ( 'NONE',  ( -8.871558582316794173, -20.24999999999999289, 3.449312527122348371 ) ) ;
#15208 = CARTESIAN_POINT ( 'NONE',  ( 7.559058582316795949, -20.19639159124062999, 5.231925497173373074 ) ) ;
#15209 = CARTESIAN_POINT ( 'NONE',  ( -9.722191417683177406, -21.02099543870834353, 3.964901035250761208 ) ) ;
#15210 = ORIENTED_EDGE ( 'NONE', *, *, #20235, .T. ) ;
#15211 = CARTESIAN_POINT ( 'NONE',  ( 13.39662663169496781, -19.15785509940297615, 5.494950532956567102 ) ) ;
#15212 = LINE ( 'NONE', #7273, #3368 ) ;
#15213 = ORIENTED_EDGE ( 'NONE', *, *, #12162, .F. ) ;
#15214 = CIRCLE ( 'NONE', #17543, 0.2500000000000002220 ) ;
#15215 = ORIENTED_EDGE ( 'NONE', *, *, #4716, .F. ) ;
#15216 = FACE_OUTER_BOUND ( 'NONE', #16345, .T. ) ;
#15217 = EDGE_LOOP ( 'NONE', ( #20693, #15309, #8149, #11209 ) ) ;
#15218 = CARTESIAN_POINT ( 'NONE',  ( -13.38921792038197900, -19.53199502070850357, 5.456033026503027017 ) ) ;
#15219 = ORIENTED_EDGE ( 'NONE', *, *, #19539, .T. ) ;
#15220 = CARTESIAN_POINT ( 'NONE',  ( 17.80017143803810242, 4.999999999999999112, 0.000000000000000000 ) ) ;
#15221 = CARTESIAN_POINT ( 'NONE',  ( -24.12918902992234393, 10.00000000000000000, 1.000000000000000000 ) ) ;
#15222 = DIRECTION ( 'NONE',  ( -0.000000000000000000, -0.000000000000000000, -1.000000000000000000 ) ) ;
#15223 = CARTESIAN_POINT ( 'NONE',  ( 3.537356407578672535, -11.36437789272258669, 3.142965222332344766 ) ) ;
#15224 = DIRECTION ( 'NONE',  ( -0.000000000000000000, -0.000000000000000000, -1.000000000000000000 ) ) ;
#15225 = AXIS2_PLACEMENT_3D ( 'NONE', #13554, #13350, #5829 ) ;
#15226 = EDGE_CURVE ( 'NONE', #9491, #13688, #9900, .T. ) ;
#15227 = CARTESIAN_POINT ( 'NONE',  ( 13.90439735423812273, 5.734566389025032684, 2.999999999999999556 ) ) ;
#15228 = DIRECTION ( 'NONE',  ( -0.000000000000000000, -0.000000000000000000, -1.000000000000000000 ) ) ;
#15229 = PLANE ( 'NONE',  #14340 ) ;
#15230 = CARTESIAN_POINT ( 'NONE',  ( 12.62844141768317741, -20.99999999999999645, 3.550687472877664952 ) ) ;
#15231 = CARTESIAN_POINT ( 'NONE',  ( -12.62499999999998224, -20.24999999999991829, 4.333333333333343695 ) ) ;
#15232 = CARTESIAN_POINT ( 'NONE',  ( -7.284691417683176518, -23.02099543870834353, 3.863526089495429972 ) ) ;
#15233 = CARTESIAN_POINT ( 'NONE',  ( -7.940941417683175629, -20.19639159124061933, 1.768074502826635586 ) ) ;
#15234 = VERTEX_POINT ( 'NONE', #5192 ) ;
#15235 = EDGE_CURVE ( 'NONE', #14114, #19732, #2359, .T. ) ;
#15236 = CARTESIAN_POINT ( 'NONE',  ( 12.70672377255832686, -15.37294948583620346, 4.840845106674187548 ) ) ;
#15237 = LINE ( 'NONE', #910, #3201 ) ;
#15238 = EDGE_LOOP ( 'NONE', ( #8329, #14407, #15001, #14389 ) ) ;
#15239 = ADVANCED_FACE ( 'NONE', ( #799 ), #11773, .T. ) ;
#15240 = CARTESIAN_POINT ( 'NONE',  ( 14.50000000000000000, -23.00000000000001421, 1.000000000000000000 ) ) ;
#15241 = LINE ( 'NONE', #13662, #19040 ) ;
#15242 = EDGE_LOOP ( 'NONE', ( #5522, #7018, #16208, #5713 ) ) ;
#15243 = ORIENTED_EDGE ( 'NONE', *, *, #13283, .T. ) ;
#15244 = ORIENTED_EDGE ( 'NONE', *, *, #16361, .T. ) ;
#15245 = DIRECTION ( 'NONE',  ( -0.000000000000000000, 0.000000000000000000, -1.000000000000000000 ) ) ;
#15246 = LINE ( 'NONE', #10341, #14639 ) ;
#15247 = CARTESIAN_POINT ( 'NONE',  ( -2.589709240944451096, -9.559844081062008669, 1.736909907557668165 ) ) ;
#15248 = DIRECTION ( 'NONE',  ( -0.000000000000000000, -0.000000000000000000, -1.000000000000000000 ) ) ;
#15249 = PLANE ( 'NONE',  #19504 ) ;
#15250 = EDGE_CURVE ( 'NONE', #16077, #11512, #15011, .T. ) ;
#15251 = CARTESIAN_POINT ( 'NONE',  ( 7.500000000000002665, -9.999999999999991118, 2.500000000000000000 ) ) ;
#15252 = CARTESIAN_POINT ( 'NONE',  ( 5.121558582316795061, -24.50000000000000000, 3.550687472877651629 ) ) ;
#15253 = CARTESIAN_POINT ( 'NONE',  ( -13.11145189917479392, 4.315820908324673688, 5.961432613039677086 ) ) ;
#15254 = CARTESIAN_POINT ( 'NONE',  ( -6.534691417683177406, -19.47900456129164581, 2.515153566944927199 ) ) ;
#15255 = VERTEX_POINT ( 'NONE', #15123 ) ;
#15256 = CARTESIAN_POINT ( 'NONE',  ( 11.30905858231679417, -23.27327832286945153, 2.298404588716537411 ) ) ;
#15257 = CARTESIAN_POINT ( 'NONE',  ( -17.55017143803810242, 9.000000000000001776, 0.000000000000000000 ) ) ;
#15258 = CARTESIAN_POINT ( 'NONE',  ( -13.89992416064626646, 5.508670112635706495, 5.888743936161951353 ) ) ;
#15259 = CARTESIAN_POINT ( 'NONE',  ( 11.21530858231679417, -23.77099543870833998, 2.825813738724734847 ) ) ;
#15260 = CARTESIAN_POINT ( 'NONE',  ( -7.626396343307448866, 11.64110105645932691, 0.000000000000000000 ) ) ;
#15261 = ORIENTED_EDGE ( 'NONE', *, *, #9150, .T. ) ;
#15262 = VERTEX_POINT ( 'NONE', #13037 ) ;
#15263 = CARTESIAN_POINT ( 'NONE',  ( 13.58606361274418184, -9.591287556442823714, 5.700679699621803209 ) ) ;
#15264 = DIRECTION ( 'NONE',  ( 0.000000000000000000, -1.000000000000000000, 0.000000000000000000 ) ) ;
#15265 = EDGE_LOOP ( 'NONE', ( #8201, #15628, #3128, #18756 ) ) ;
#15266 = PLANE ( 'NONE',  #9789 ) ;
#15267 = DIRECTION ( 'NONE',  ( 0.000000000000000000, -0.000000000000000000, 1.000000000000000000 ) ) ;
#15268 = DIRECTION ( 'NONE',  ( -0.000000000000000000, 0.000000000000000000, -1.000000000000000000 ) ) ;
#15269 = DIRECTION ( 'NONE',  ( 5.782411586589356653E-16, -1.000000000000000000, 0.000000000000000000 ) ) ;
#15270 = CARTESIAN_POINT ( 'NONE',  ( 0.000000000000000000, 9.000000000000001776, 1.000000000000000000 ) ) ;
#15271 = CARTESIAN_POINT ( 'NONE',  ( 3.385922596301560894, -9.481287983549590237, 1.909350115156127403 ) ) ;
#15272 = CIRCLE ( 'NONE', #17619, 59.99999999999998579 ) ;
#15273 = EDGE_CURVE ( 'NONE', #886, #14781, #3620, .T. ) ;
#15274 = ADVANCED_FACE ( 'NONE', ( #4038 ), #7281, .T. ) ;
#15275 = DIRECTION ( 'NONE',  ( 0.000000000000000000, 0.000000000000000000, 1.000000000000000000 ) ) ;
#15276 = CARTESIAN_POINT ( 'NONE',  ( -13.09300823383486900, 4.134415808666423331, 5.226944302881396887 ) ) ;
#15277 = CARTESIAN_POINT ( 'NONE',  ( 10.65280858231679240, -21.22443879296942626, 5.229004561291659137 ) ) ;
#15278 = CARTESIAN_POINT ( 'NONE',  ( -13.86796007304617717, 3.894483688830428836, 6.740724019197413597 ) ) ;
#15279 = EDGE_CURVE ( 'NONE', #4668, #6506, #4242, .T. ) ;
#15280 = PLANE ( 'NONE',  #7718 ) ;
#15281 = CARTESIAN_POINT ( 'NONE',  ( 10.55905858231679595, -20.72672167713054137, 4.701595411283463477 ) ) ;
#15282 = CARTESIAN_POINT ( 'NONE',  ( 12.25344141768317741, -21.94931252712233061, 2.499999999999999112 ) ) ;
#15283 = CARTESIAN_POINT ( 'NONE',  ( -9.246558582316794173, -21.94931252712234482, 5.250000000000000888 ) ) ;
#15284 = ORIENTED_EDGE ( 'NONE', *, *, #17331, .F. ) ;
#15285 = CARTESIAN_POINT ( 'NONE',  ( 12.62691554569741648, -19.40326494227377907, 4.703927990036796736 ) ) ;
#15286 = LINE ( 'NONE', #15084, #17019 ) ;
#15287 = ORIENTED_EDGE ( 'NONE', *, *, #11261, .T. ) ;
#15288 = VECTOR ( 'NONE', #9407, 1000.000000000000000 ) ;
#15289 = ADVANCED_FACE ( 'NONE', ( #7181 ), #15431, .T. ) ;
#15290 = ORIENTED_EDGE ( 'NONE', *, *, #5819, .T. ) ;
#15291 = CARTESIAN_POINT ( 'NONE',  ( 15.00000000000000355, -30.00000000000000000, 0.000000000000000000 ) ) ;
#15292 = CARTESIAN_POINT ( 'NONE',  ( -12.91308523408712183, -5.701695678577235249, 5.798858176249892082 ) ) ;
#15293 = CARTESIAN_POINT ( 'NONE',  ( -3.047379876266447685, -13.13734219723468755, 3.405682891496055742 ) ) ;
#15294 = CARTESIAN_POINT ( 'NONE',  ( -13.84983662433050178, 3.729249528687784920, 5.987138032956566214 ) ) ;
#15295 = VECTOR ( 'NONE', #15329, 1000.000000000000000 ) ;
#15296 = CARTESIAN_POINT ( 'NONE',  ( -7.626396343307448866, 11.64110105645932691, 10.00000000000000000 ) ) ;
#15297 = CARTESIAN_POINT ( 'NONE',  ( 1.407845757905374695, -9.114917468222230923, 2.372643865078341019 ) ) ;
#15298 = DIRECTION ( 'NONE',  ( -1.000000000000000000, 0.000000000000000000, 0.000000000000000000 ) ) ;
#15299 = PLANE ( 'NONE',  #15739 ) ;
#15300 = VECTOR ( 'NONE', #14084, 1000.000000000000000 ) ;
#15301 = DIRECTION ( 'NONE',  ( 1.000000000000000000, -0.000000000000000000, -0.000000000000000000 ) ) ;
#15302 = CARTESIAN_POINT ( 'NONE',  ( -10.18405858231679595, -20.26807450282662160, 1.696391591240633101 ) ) ;
#15303 = CARTESIAN_POINT ( 'NONE',  ( -3.462011766956747394, -14.92507028461178287, 3.114807177791267812 ) ) ;
#15304 = VERTEX_POINT ( 'NONE', #12187 ) ;
#15305 = CARTESIAN_POINT ( 'NONE',  ( -13.37500751150753864, -19.49962066887028556, 4.515663405036051792 ) ) ;
#15306 = CARTESIAN_POINT ( 'NONE',  ( -7.626396343307448866, 16.00000000000000000, 1.000000000000000000 ) ) ;
#15307 = CARTESIAN_POINT ( 'NONE',  ( 11.87844141768317741, -24.50000000000000000, 3.449312527122335048 ) ) ;
#15308 = CARTESIAN_POINT ( 'NONE',  ( -8.222191417683175629, -21.02099543870834353, 3.964901035250761208 ) ) ;
#15309 = ORIENTED_EDGE ( 'NONE', *, *, #10313, .F. ) ;
#15310 = CARTESIAN_POINT ( 'NONE',  ( 13.44218742460511073, -16.85703505742523234, 5.544429699623282914 ) ) ;
#15311 = CARTESIAN_POINT ( 'NONE',  ( 0.000000000000000000, 9.000000000000001776, 1.000000000000000000 ) ) ;
#15312 = ORIENTED_EDGE ( 'NONE', *, *, #6279, .T. ) ;
#15313 = VERTEX_POINT ( 'NONE', #5604 ) ;
#15314 = EDGE_CURVE ( 'NONE', #16322, #13679, #4139, .T. ) ;
#15315 = DIRECTION ( 'NONE',  ( 1.000000000000000000, -2.312964634635752916E-15, 0.000000000000000000 ) ) ;
#15316 = VECTOR ( 'NONE', #14010, 1000.000000000000000 ) ;
#15317 = ORIENTED_EDGE ( 'NONE', *, *, #7719, .T. ) ;
#15318 = CARTESIAN_POINT ( 'NONE',  ( -13.87367531042247748, 4.933103176334663331, 5.324010972534209074 ) ) ;
#15319 = ORIENTED_EDGE ( 'NONE', *, *, #690, .T. ) ;
#15320 = CARTESIAN_POINT ( 'NONE',  ( -3.497260319564023057, 4.999999999999999112, 1.000000000000000000 ) ) ;
#15321 = LINE ( 'NONE', #19948, #19702 ) ;
#15322 = AXIS2_PLACEMENT_3D ( 'NONE', #9286, #20500, #4578 ) ;
#15323 = LINE ( 'NONE', #1003, #10994 ) ;
#15324 = AXIS2_PLACEMENT_3D ( 'NONE', #19949, #7184, #15125 ) ;
#15325 = CARTESIAN_POINT ( 'NONE',  ( 3.034277558025862298, -9.029550313327863620, 2.543334857076493094 ) ) ;
#15326 = CARTESIAN_POINT ( 'NONE',  ( -7.369520639128046113, 0.000000000000000000, 1.000000000000000000 ) ) ;
#15327 = CARTESIAN_POINT ( 'NONE',  ( 12.65017171054692113, -19.72882861737994631, 6.192581331858542981 ) ) ;
#15328 = AXIS2_PLACEMENT_3D ( 'NONE', #1162, #20521, #15480 ) ;
#15329 = DIRECTION ( 'NONE',  ( -0.000000000000000000, -0.000000000000000000, -1.000000000000000000 ) ) ;
#15330 = DIRECTION ( 'NONE',  ( -0.000000000000000000, -0.000000000000000000, -1.000000000000000000 ) ) ;
#15331 = CARTESIAN_POINT ( 'NONE',  ( 13.12529397354238192, 5.014845663890295846, 4.916666666666650087 ) ) ;
#15332 = CARTESIAN_POINT ( 'NONE',  ( 5.503441417683176518, -22.05068747287765873, 5.250000000000000888 ) ) ;
#15333 = DIRECTION ( 'NONE',  ( 0.000000000000000000, -1.000000000000000000, 0.000000000000000000 ) ) ;
#15334 = CARTESIAN_POINT ( 'NONE',  ( -13.27780858231679417, -21.02099543870833998, 3.035098964749253003 ) ) ;
#15335 = CARTESIAN_POINT ( 'NONE',  ( -9.440941417683177406, -20.19639159124061933, 1.768074502826635586 ) ) ;
#15336 = VERTEX_POINT ( 'NONE', #895 ) ;
#15337 = CARTESIAN_POINT ( 'NONE',  ( 12.62500000000002132, -19.50000000000273559, 4.083333333315724012 ) ) ;
#15338 = CARTESIAN_POINT ( 'NONE',  ( -13.12119116326504908, 4.807653744879115010, 5.626470997801169105 ) ) ;
#15339 = ORIENTED_EDGE ( 'NONE', *, *, #17030, .F. ) ;
#15340 = DIRECTION ( 'NONE',  ( 0.000000000000000000, 0.000000000000000000, 1.000000000000000000 ) ) ;
#15341 = CARTESIAN_POINT ( 'NONE',  ( 0.000000000000000000, 4.999999999999999112, 1.000000000000000000 ) ) ;
#15342 = EDGE_LOOP ( 'NONE', ( #16481, #18419, #15261, #5753 ) ) ;
#15343 = CARTESIAN_POINT ( 'NONE',  ( 1.903957340438703572, -10.27085516675799148, 2.476896775482616331 ) ) ;
#15344 = CONTEXT_DEPENDENT_SHAPE_REPRESENTATION ( #16167, #12335 ) ;
#15345 = ORIENTED_EDGE ( 'NONE', *, *, #3340, .T. ) ;
#15346 = EDGE_CURVE ( 'NONE', #14595, #15669, #20359, .T. ) ;
#15347 = AXIS2_PLACEMENT_3D ( 'NONE', #5738, #14926, #10542 ) ;
#15348 = VERTEX_POINT ( 'NONE', #13642 ) ;
#15349 = CARTESIAN_POINT ( 'NONE',  ( 0.000000000000000000, 10.00000000000000000, 1.000000000000000000 ) ) ;
#15350 = DIRECTION ( 'NONE',  ( 1.000000000000000000, -0.000000000000000000, 0.000000000000000000 ) ) ;
#15351 = VECTOR ( 'NONE', #1803, 1000.000000000000000 ) ;
#15352 = CARTESIAN_POINT ( 'NONE',  ( -1.897597015127918230, -9.924601616748528699, 1.637971946730535588 ) ) ;
#15353 = LINE ( 'NONE', #20188, #8036 ) ;
#15354 = CARTESIAN_POINT ( 'NONE',  ( 7.619520639128047002, 9.000000000000001776, 0.000000000000000000 ) ) ;
#15355 = EDGE_CURVE ( 'NONE', #11612, #9195, #10423, .T. ) ;
#15356 = CARTESIAN_POINT ( 'NONE',  ( -13.50000000000000178, 5.000000000000047962, 4.000000000000000000 ) ) ;
#15357 = VECTOR ( 'NONE', #7969, 1000.000000000000000 ) ;
#15358 = CARTESIAN_POINT ( 'NONE',  ( 11.78469141768317741, -24.52099543870834708, 4.484846433055073689 ) ) ;
#15359 = CARTESIAN_POINT ( 'NONE',  ( -13.12270769621861355, 4.884238659038159902, 5.513847264053151065 ) ) ;
#15360 = CARTESIAN_POINT ( 'NONE',  ( -5.878441417683177406, -24.50000000000000000, 3.449312527122335048 ) ) ;
#15361 = VERTEX_POINT ( 'NONE', #17104 ) ;
#15362 = CARTESIAN_POINT ( 'NONE',  ( 11.12155858231679417, -23.74999999999999645, 3.550687472877651629 ) ) ;
#15363 = LINE ( 'NONE', #8791, #10751 ) ;
#15364 = CARTESIAN_POINT ( 'NONE',  ( -13.88045627189955233, 4.525541730927888473, 6.662882075361062029 ) ) ;
#15365 = AXIS2_PLACEMENT_3D ( 'NONE', #1522, #19208, #14266 ) ;
#15366 = CARTESIAN_POINT ( 'NONE',  ( 5.402808582316795949, -22.46490103525074034, 2.520995438708341307 ) ) ;
#15367 = CARTESIAN_POINT ( 'NONE',  ( 0.000000000000000000, 0.000000000000000000, 1.000000000000000000 ) ) ;
#15368 = EDGE_LOOP ( 'NONE', ( #11678, #19318, #7892, #9159 ) ) ;
#15369 = ORIENTED_EDGE ( 'NONE', *, *, #15577, .F. ) ;
#15370 = CARTESIAN_POINT ( 'NONE',  ( 13.42793873098995938, -18.32659408500397191, 6.262859435864284841 ) ) ;
#15371 = DIRECTION ( 'NONE',  ( -0.000000000000000000, -0.000000000000000000, -1.000000000000000000 ) ) ;
#15372 = VERTEX_POINT ( 'NONE', #1115 ) ;
#15373 = ADVANCED_FACE ( 'NONE', ( #13853 ), #2462, .T. ) ;
#15374 = DIRECTION ( 'NONE',  ( -0.1351665943404259662, -0.9596796555888893465, 0.2464649070825324084 ) ) ;
#15375 = VECTOR ( 'NONE', #17182, 1000.000000000000000 ) ;
#15376 = VECTOR ( 'NONE', #3857, 1000.000000000000000 ) ;
#15377 = ORIENTED_EDGE ( 'NONE', *, *, #3593, .T. ) ;
#15378 = CARTESIAN_POINT ( 'NONE',  ( -12.15280858231679595, -21.22443879296942626, 5.229004561291659137 ) ) ;
#15379 = CARTESIAN_POINT ( 'NONE',  ( 13.87066368810231154, 4.781016249162736820, 5.617237349937618696 ) ) ;
#15380 = CARTESIAN_POINT ( 'NONE',  ( -14.49999999999999645, -22.99999999999998579, 4.000000000000000000 ) ) ;
#15381 = CARTESIAN_POINT ( 'NONE',  ( 3.451003380014874722, -9.682417022083358304, 1.961004070207825523 ) ) ;
#15382 = AXIS2_PLACEMENT_3D ( 'NONE', #8127, #13227, #19531 ) ;
#15383 = VECTOR ( 'NONE', #5923, 1000.000000000000000 ) ;
#15384 = LINE ( 'NONE', #2837, #11066 ) ;
#15385 = CARTESIAN_POINT ( 'NONE',  ( -13.08739618700683849, 3.851007443844064237, 5.254256565007597857 ) ) ;
#15386 = CARTESIAN_POINT ( 'NONE',  ( 10.55905858231679595, -20.72672167713054137, 4.701595411283463477 ) ) ;
#15387 = CARTESIAN_POINT ( 'NONE',  ( -13.39782821820594627, -19.84717498059871943, 6.143582220458365661 ) ) ;
#15388 = DIRECTION ( 'NONE',  ( 1.000000000000000000, 0.000000000000000000, 0.000000000000000000 ) ) ;
#15389 = CARTESIAN_POINT ( 'NONE',  ( 12.90280858231679773, -22.77556120703056308, 1.770995438708339975 ) ) ;
#15390 = CARTESIAN_POINT ( 'NONE',  ( 5.128441417683177406, -20.24999999999999289, 3.550687472877664952 ) ) ;
#15391 = CARTESIAN_POINT ( 'NONE',  ( -8.590308582316794173, -21.32581373872472597, 1.729004561291657582 ) ) ;
#15392 = EDGE_LOOP ( 'NONE', ( #5214, #17324, #13274, #10472 ) ) ;
#15393 = CARTESIAN_POINT ( 'NONE',  ( 13.38210008768272630, -19.14144557202113006, 4.745270796715706396 ) ) ;
#15394 = LINE ( 'NONE', #4003, #10350 ) ;
#15395 = VERTEX_POINT ( 'NONE', #15220 ) ;
#15396 = ADVANCED_FACE ( 'NONE', ( #20052 ), #9060, .T. ) ;
#15397 = VECTOR ( 'NONE', #20132, 1000.000000000000114 ) ;
#15398 = ORIENTED_EDGE ( 'NONE', *, *, #16071, .T. ) ;
#15399 = EDGE_CURVE ( 'NONE', #1461, #12022, #9160, .T. ) ;
#15400 = CARTESIAN_POINT ( 'NONE',  ( 26.04469207716615031, 0.000000000000000000, 1.000000000000000000 ) ) ;
#15401 = CARTESIAN_POINT ( 'NONE',  ( -12.66369984131459070, -18.29565801360988075, 5.528024842915327142 ) ) ;
#15402 = CARTESIAN_POINT ( 'NONE',  ( -2.602174906157317835, -9.976397331638239052, 2.593889103792902606 ) ) ;
#15403 = CARTESIAN_POINT ( 'NONE',  ( -13.47096266223369376, -15.40388555723029462, 5.575679699623145247 ) ) ;
#15404 = DIRECTION ( 'NONE',  ( 0.000000000000000000, 0.1264857625231113059, -0.9919684228235025047 ) ) ;
#15405 = CARTESIAN_POINT ( 'NONE',  ( -0.000000000000000000, 10.00000000000000000, 0.000000000000000000 ) ) ;
#15406 = CARTESIAN_POINT ( 'NONE',  ( 2.311130159782011972, 4.999999999999999112, 1.000000000000000000 ) ) ;
#15407 = DIRECTION ( 'NONE',  ( 0.000000000000000000, -0.000000000000000000, 1.000000000000000000 ) ) ;
#15408 = ADVANCED_FACE ( 'NONE', ( #7590 ), #12087, .F. ) ;
#15409 = VECTOR ( 'NONE', #1707, 1000.000000000000000 ) ;
#15410 = CARTESIAN_POINT ( 'NONE',  ( 4.509702210102195075, -21.45583770899529696, 5.512481659358018149 ) ) ;
#15411 = CARTESIAN_POINT ( 'NONE',  ( -9.246558582316795949, -21.94931252712234127, 6.000000000000001776 ) ) ;
#15412 = CARTESIAN_POINT ( 'NONE',  ( -1.407845757905374695, -8.364917468222230923, 1.622643865078341907 ) ) ;
#15413 = VERTEX_POINT ( 'NONE', #10732 ) ;
#15414 = CARTESIAN_POINT ( 'NONE',  ( -13.37524505148396514, -20.23762490005974968, 4.659512268729234741 ) ) ;
#15415 = PLANE ( 'NONE',  #18410 ) ;
#15416 = CARTESIAN_POINT ( 'NONE',  ( 5.684058582316795949, -20.26807450282662160, 1.696391591240633101 ) ) ;
#15417 = CARTESIAN_POINT ( 'NONE',  ( -7.753441417683177406, -21.94931252712233061, 2.499999999999999112 ) ) ;
#15418 = ORIENTED_EDGE ( 'NONE', *, *, #5623, .T. ) ;
#15419 = CARTESIAN_POINT ( 'NONE',  ( 13.43259567872942917, -17.34141822415733714, 5.534013032956523581 ) ) ;
#15420 = FACE_OUTER_BOUND ( 'NONE', #18422, .T. ) ;
#15421 = EDGE_LOOP ( 'NONE', ( #14974, #7356, #172, #4671 ) ) ;
#15422 = VERTEX_POINT ( 'NONE', #13754 ) ;
#15423 = DIRECTION ( 'NONE',  ( -6.938893903907222067E-15, -1.000000000000000000, 0.000000000000000000 ) ) ;
#15424 = EDGE_CURVE ( 'NONE', #4929, #13278, #13955, .T. ) ;
#15425 = EDGE_LOOP ( 'NONE', ( #17049, #3565, #5004, #9800 ) ) ;
#15426 = EDGE_CURVE ( 'NONE', #1844, #4979, #17204, .T. ) ;
#15427 = CARTESIAN_POINT ( 'NONE',  ( -13.87470602645761986, 4.985154336109792972, 4.666666666666619889 ) ) ;
#15428 = VECTOR ( 'NONE', #7430, 1000.000000000000000 ) ;
#15429 = CARTESIAN_POINT ( 'NONE',  ( -3.497260319564023057, 0.000000000000000000, 0.000000000000000000 ) ) ;
#15430 = ORIENTED_EDGE ( 'NONE', *, *, #16707, .F. ) ;
#15431 = CYLINDRICAL_SURFACE ( 'NONE', #9000, 10.00000000000000000 ) ;
#15432 = DIRECTION ( 'NONE',  ( -0.000000000000000000, -0.000000000000000000, -1.000000000000000000 ) ) ;
#15433 = MECHANICAL_DESIGN_GEOMETRIC_PRESENTATION_REPRESENTATION (  '', ( #12756 ), #6917 ) ;
#15434 = PLANE ( 'NONE',  #983 ) ;
#15435 = CARTESIAN_POINT ( 'NONE',  ( 2.121089610268797276, -8.411987239090384705, 1.634732322550447758 ) ) ;
#15436 = LINE ( 'NONE', #18582, #514 ) ;
#15437 = CARTESIAN_POINT ( 'NONE',  ( 13.10431844137356627, 3.955581289335645234, 6.006545679920360925 ) ) ;
#15438 = ADVANCED_FACE ( 'NONE', ( #15629 ), #13545, .T. ) ;
#15439 = LINE ( 'NONE', #1426, #20351 ) ;
#15440 = LINE ( 'NONE', #9167, #19744 ) ;
#15441 = CARTESIAN_POINT ( 'NONE',  ( 13.12529397353891270, 5.014845663890295846, 3.333333333333220239 ) ) ;
#15442 = CARTESIAN_POINT ( 'NONE',  ( 8.409691417683177406, -21.63647391050456648, 4.520995438708348857 ) ) ;
#15443 = CYLINDRICAL_SURFACE ( 'NONE', #3542, 10.00000000000000000 ) ;
#15444 = CARTESIAN_POINT ( 'NONE',  ( -12.52780858231679773, -22.97900456129165647, 3.964901035250747885 ) ) ;
#15445 = CARTESIAN_POINT ( 'NONE',  ( -7.847191417683175629, -20.91377862118959285, 1.020995438708345082 ) ) ;
#15446 = ORIENTED_EDGE ( 'NONE', *, *, #3222, .T. ) ;
#15447 = CARTESIAN_POINT ( 'NONE',  ( 12.62499999999998224, -19.49999999999991473, 4.333333333333343695 ) ) ;
#15448 = CARTESIAN_POINT ( 'NONE',  ( -12.64931222250080545, -19.02223276370786209, 5.512399842915133519 ) ) ;
#15449 = ORIENTED_EDGE ( 'NONE', *, *, #4954, .T. ) ;
#15450 = DIRECTION ( 'NONE',  ( 1.000000000000000000, 0.000000000000000000, 0.000000000000000000 ) ) ;
#15451 = ORIENTED_EDGE ( 'NONE', *, *, #19919, .F. ) ;
#15452 = CARTESIAN_POINT ( 'NONE',  ( 1.824488249492779879, -9.124319963227819130, 2.375058613629473570 ) ) ;
#15453 = ORIENTED_EDGE ( 'NONE', *, *, #2460, .T. ) ;
#15454 = PLANE ( 'NONE',  #17666 ) ;
#15455 = VECTOR ( 'NONE', #9635, 1000.000000000000000 ) ;
#15456 = CARTESIAN_POINT ( 'NONE',  ( -11.00000000000000000, -18.49999999999999645, 4.000000000000000000 ) ) ;
#15457 = CARTESIAN_POINT ( 'NONE',  ( -1.126276606324276619, -9.114917468222230923, 1.622643865078341463 ) ) ;
#15458 = CARTESIAN_POINT ( 'NONE',  ( -26.94203811574920593, 10.00000000000000000, 1.000000000000000000 ) ) ;
#15459 = CARTESIAN_POINT ( 'NONE',  ( 15.50000000000001776, -17.49999999999999645, 1.000000000000000000 ) ) ;
#15460 = CARTESIAN_POINT ( 'NONE',  ( -1.561130159782011306, 4.999999999999999112, 1.000000000000000000 ) ) ;
#15461 = CARTESIAN_POINT ( 'NONE',  ( 12.25344141768317741, -21.94931252712233061, 0.9999999999999978906 ) ) ;
#15462 = CARTESIAN_POINT ( 'NONE',  ( -13.10624331898488037, 4.052787608736739600, 6.006964772046813117 ) ) ;
#15463 = CARTESIAN_POINT ( 'NONE',  ( -12.15969141768317741, -22.67418626127524917, 1.729004561291651809 ) ) ;
#15464 = EDGE_CURVE ( 'NONE', #10048, #6813, #20156, .T. ) ;
#15465 = AXIS2_PLACEMENT_3D ( 'NONE', #14740, #416, #6797 ) ;
#15466 = EDGE_LOOP ( 'NONE', ( #13736, #10220, #19653, #13256 ) ) ;
#15467 = CARTESIAN_POINT ( 'NONE',  ( 3.747260319564023501, 4.999999999999999112, 1.000000000000000000 ) ) ;
#15468 = CARTESIAN_POINT ( 'NONE',  ( -3.997260319564023501, 4.999999999999999112, 1.000000000000000000 ) ) ;
#15469 = CARTESIAN_POINT ( 'NONE',  ( -13.84997554952896515, 2.986265251207539606, 6.721192769197450012 ) ) ;
#15470 = VECTOR ( 'NONE', #4700, 1000.000000000000000 ) ;
#15471 = CARTESIAN_POINT ( 'NONE',  ( 4.687312169500634340, -21.70215802671379990, 4.455959925339818106 ) ) ;
#15472 = CARTESIAN_POINT ( 'NONE',  ( 14.31494360078803041, 0.000000000000000000, 0.000000000000000000 ) ) ;
#15473 = ORIENTED_EDGE ( 'NONE', *, *, #17592, .F. ) ;
#15474 = ORIENTED_EDGE ( 'NONE', *, *, #13743, .T. ) ;
#15475 = CARTESIAN_POINT ( 'NONE',  ( 13.39995901559228031, -19.73956971259024229, 6.178279423016713956 ) ) ;
#15476 = DIRECTION ( 'NONE',  ( 1.000000000000000000, 0.000000000000000000, 0.000000000000000000 ) ) ;
#15477 = ORIENTED_EDGE ( 'NONE', *, *, #1314, .T. ) ;
#15478 = CARTESIAN_POINT ( 'NONE',  ( 23.10856191738414012, 9.000000000000001776, 0.000000000000000000 ) ) ;
#15479 = ORIENTED_EDGE ( 'NONE', *, *, #13085, .F. ) ;
#15480 = DIRECTION ( 'NONE',  ( 0.000000000000000000, 0.000000000000000000, -1.000000000000000000 ) ) ;
#15481 = CARTESIAN_POINT ( 'NONE',  ( 26.69203811574920948, 1.543443504701929706E-14, 1.000000000000000000 ) ) ;
#15482 = DIRECTION ( 'NONE',  ( -0.000000000000000000, -0.000000000000000000, -1.000000000000000000 ) ) ;
#15483 = CARTESIAN_POINT ( 'NONE',  ( 3.549867680106858714, -10.29705900472337632, 2.118856410057032402 ) ) ;
#15484 = CARTESIAN_POINT ( 'NONE',  ( 23.10856191738414012, 4.999999999999999112, 1.000000000000000000 ) ) ;
#15485 = CARTESIAN_POINT ( 'NONE',  ( -13.37499999999998401, -19.49999999999998934, 3.666666666666654084 ) ) ;
#15486 = CARTESIAN_POINT ( 'NONE',  ( 13.27780858231679595, -20.27099543870833642, 2.724438792969431589 ) ) ;
#15487 = CARTESIAN_POINT ( 'NONE',  ( -13.42793873098995938, -18.32659408500397191, 6.262859435864284841 ) ) ;
#15488 = EDGE_CURVE ( 'NONE', #18502, #17840, #13090, .T. ) ;
#15489 = CARTESIAN_POINT ( 'NONE',  ( -2.061130159782011972, 0.000000000000000000, 1.000000000000000000 ) ) ;
#15490 = CARTESIAN_POINT ( 'NONE',  ( 12.15280858231679595, -21.22443879296942626, 5.229004561291659137 ) ) ;
#15491 = CARTESIAN_POINT ( 'NONE',  ( 12.15969141768317918, -22.36352608949543352, 2.479004561291652031 ) ) ;
#15492 = CARTESIAN_POINT ( 'NONE',  ( -7.465308582316795061, -20.22900456129164937, 4.174186261275266929 ) ) ;
#15493 = ORIENTED_EDGE ( 'NONE', *, *, #809, .T. ) ;
#15494 = EDGE_CURVE ( 'NONE', #19407, #15727, #19385, .T. ) ;
#15495 = CARTESIAN_POINT ( 'NONE',  ( 13.37499999999998401, -19.49999999999998934, 3.666666666666654084 ) ) ;
#15496 = ADVANCED_FACE ( 'NONE', ( #5044 ), #6325, .T. ) ;
#15497 = CARTESIAN_POINT ( 'NONE',  ( -20.00000000000000000, 0.000000000000000000, 2.000000000000000000 ) ) ;
#15498 = ORIENTED_EDGE ( 'NONE', *, *, #10836, .F. ) ;
#15499 = UNCERTAINTY_MEASURE_WITH_UNIT (LENGTH_MEASURE( 1.000000000000000082E-05 ), #19458, 'distance_accuracy_value', 'NONE');
#15500 = VERTEX_POINT ( 'NONE', #15737 ) ;
#15501 = DIRECTION ( 'NONE',  ( 1.000000000000000000, 0.000000000000000000, 0.000000000000000000 ) ) ;
#15502 = CARTESIAN_POINT ( 'NONE',  ( -13.10431844137356627, 3.955581289335645234, 6.006545679920360925 ) ) ;
#15503 = CARTESIAN_POINT ( 'NONE',  ( 10.05565079891005631, 4.999999999999999112, 1.000000000000000000 ) ) ;
#15504 = CARTESIAN_POINT ( 'NONE',  ( -13.39722611581222189, -19.12758115148224647, 5.495601574623241170 ) ) ;
#15505 = CARTESIAN_POINT ( 'NONE',  ( -14.49999999999998579, -24.49999999999999289, 4.000000000000000000 ) ) ;
#15506 = DIRECTION ( 'NONE',  ( 0.000000000000000000, 0.000000000000000000, -1.000000000000000000 ) ) ;
#15507 = CARTESIAN_POINT ( 'NONE',  ( -15.00000000000000000, 3.000000000000000000, 1.000000000000000000 ) ) ;
#15508 = CARTESIAN_POINT ( 'NONE',  ( 0.000000000000000000, 10.00000000000000000, 1.000000000000000000 ) ) ;
#15509 = EDGE_CURVE ( 'NONE', #7326, #6555, #14656, .T. ) ;
#15510 = CARTESIAN_POINT ( 'NONE',  ( -24.12918902992234393, 0.000000000000000000, 1.000000000000000000 ) ) ;
#15511 = CARTESIAN_POINT ( 'NONE',  ( -8.121558582316795949, -24.50000000000000000, 3.550687472877651629 ) ) ;
#15512 = CARTESIAN_POINT ( 'NONE',  ( -1.906542528716098417, -8.376716462152538512, 1.625674082428238298 ) ) ;
#15513 = ORIENTED_EDGE ( 'NONE', *, *, #8097, .T. ) ;
#15514 = CARTESIAN_POINT ( 'NONE',  ( -13.84167967300649238, 4.067323486828401613, 5.231641758301140754 ) ) ;
#15515 = PLANE ( 'NONE',  #7046 ) ;
#15516 = CARTESIAN_POINT ( 'NONE',  ( 4.840308582316795061, -22.98484643305508612, 6.020995438708344416 ) ) ;
#15517 = CARTESIAN_POINT ( 'NONE',  ( -4.753441417683176518, -21.94931252712233061, 2.499999999999999112 ) ) ;
#15518 = VERTEX_POINT ( 'NONE', #5144 ) ;
#15519 = CARTESIAN_POINT ( 'NONE',  ( 13.87470602645761986, 4.985154336109792972, 4.833333333333344584 ) ) ;
#15520 = CARTESIAN_POINT ( 'NONE',  ( 12.63249216759192350, -19.87164553660301536, 5.297612231341934041 ) ) ;
#15521 = VERTEX_POINT ( 'NONE', #7801 ) ;
#15522 = ORIENTED_EDGE ( 'NONE', *, *, #13573, .T. ) ;
#15523 = DIRECTION ( 'NONE',  ( 1.000000000000000000, -0.000000000000000000, 0.000000000000000000 ) ) ;
#15524 = EDGE_LOOP ( 'NONE', ( #16881, #10616, #6887, #2637 ) ) ;
#15525 = CARTESIAN_POINT ( 'NONE',  ( -13.40022353639839103, -18.97621141187856608, 5.498856782956575984 ) ) ;
#15526 = EDGE_CURVE ( 'NONE', #10023, #14414, #9849, .T. ) ;
#15527 = CARTESIAN_POINT ( 'NONE',  ( -13.58954612507874238, -0.5000000000000004441, 1.000000000000000000 ) ) ;
#15528 = ORIENTED_EDGE ( 'NONE', *, *, #13257, .F. ) ;
#15529 = DIRECTION ( 'NONE',  ( 0.000000000000000000, 0.000000000000000000, -1.000000000000000000 ) ) ;
#15530 = CARTESIAN_POINT ( 'NONE',  ( 9.555650798910054533, 4.999999999999999112, 0.000000000000000000 ) ) ;
#15531 = VECTOR ( 'NONE', #159, 1000.000000000000000 ) ;
#15532 = ADVANCED_BREP_SHAPE_REPRESENTATION ( '', ( #10862, #18039 ), #19052 ) ;
#15533 = DIRECTION ( 'NONE',  ( 0.000000000000000000, -1.000000000000000000, 0.000000000000000000 ) ) ;
#15534 = CARTESIAN_POINT ( 'NONE',  ( 3.528325504133930313, -10.14411005961392398, 2.079576065490765124 ) ) ;
#15535 = CARTESIAN_POINT ( 'NONE',  ( -8.376396343307449754, 10.00000000000000000, 0.000000000000000000 ) ) ;
#15536 = DIRECTION ( 'NONE',  ( 1.000000000000000000, 0.000000000000000000, 0.000000000000000000 ) ) ;
#15537 = EDGE_CURVE ( 'NONE', #3029, #1688, #8394, .T. ) ;
#15538 = CARTESIAN_POINT ( 'NONE',  ( 13.92791111847407848, 9.000000000000001776, 1.000000000000000000 ) ) ;
#15539 = LINE ( 'NONE', #5826, #16383 ) ;
#15540 = EDGE_CURVE ( 'NONE', #20714, #13339, #2007, .T. ) ;
#15541 = LINE ( 'NONE', #10629, #6373 ) ;
#15542 = AXIS2_PLACEMENT_3D ( 'NONE', #5556, #13286, #750 ) ;
#15543 = CIRCLE ( 'NONE', #15882, 0.3750000000000003331 ) ;
#15544 = CARTESIAN_POINT ( 'NONE',  ( 7.847191417683175629, -21.53509896474923835, 2.520995438708346192 ) ) ;
#15545 = CARTESIAN_POINT ( 'NONE',  ( -13.11740841389447709, 4.616624901677048420, 5.813473370769506765 ) ) ;
#15546 = CARTESIAN_POINT ( 'NONE',  ( -10.65280858231679595, -21.53509896474924901, 4.479004561291659137 ) ) ;
#15547 = CARTESIAN_POINT ( 'NONE',  ( -11.03469141768317741, -19.47900456129164581, 2.515153566944927199 ) ) ;
#15548 = ORIENTED_EDGE ( 'NONE', *, *, #11713, .F. ) ;
#15549 = CARTESIAN_POINT ( 'NONE',  ( 13.09560264576187905, 4.265433610975056133, 4.583333333333295734 ) ) ;
#15550 = CARTESIAN_POINT ( 'NONE',  ( 15.86404127825609400, 9.000000000000001776, 1.000000000000000000 ) ) ;
#15551 = ORIENTED_EDGE ( 'NONE', *, *, #16334, .F. ) ;
#15552 = LINE ( 'NONE', #19223, #17649 ) ;
#15553 = EDGE_LOOP ( 'NONE', ( #12307, #8736, #15551, #4477 ) ) ;
#15554 = CARTESIAN_POINT ( 'NONE',  ( 1.407845757905374695, -9.864917468222230923, 2.372643865078341019 ) ) ;
#15555 = EDGE_CURVE ( 'NONE', #1608, #12080, #17805, .T. ) ;
#15556 = ORIENTED_EDGE ( 'NONE', *, *, #20468, .F. ) ;
#15557 = CARTESIAN_POINT ( 'NONE',  ( 0.000000000000000000, 0.000000000000000000, 0.000000000000000000 ) ) ;
#15558 = DIRECTION ( 'NONE',  ( 1.000000000000000000, -0.000000000000000000, 0.000000000000000000 ) ) ;
#15559 = CARTESIAN_POINT ( 'NONE',  ( -2.512468814886674284, -13.43512376012158782, 2.539544162874482591 ) ) ;
#15560 = DIRECTION ( 'NONE',  ( -1.000000000000000000, 0.000000000000000000, -0.000000000000000000 ) ) ;
#15561 = DIRECTION ( 'NONE',  ( 0.000000000000000000, -1.000000000000000000, 0.000000000000000000 ) ) ;
#15562 = DIRECTION ( 'NONE',  ( 1.000000000000000000, -0.000000000000000000, -0.000000000000000000 ) ) ;
#15563 = CARTESIAN_POINT ( 'NONE',  ( 5.784691417683178294, -24.52099543870834708, 4.484846433055073689 ) ) ;
#15564 = DIRECTION ( 'NONE',  ( 0.000000000000000000, 1.000000000000000000, 0.000000000000000000 ) ) ;
#15565 = CARTESIAN_POINT ( 'NONE',  ( -9.347191417683177406, -21.22443879296941915, 1.770995438708345748 ) ) ;
#15566 = ORIENTED_EDGE ( 'NONE', *, *, #8470, .T. ) ;
#15567 = CARTESIAN_POINT ( 'NONE',  ( 8.402808582316794173, -22.77556120703056308, 1.770995438708339975 ) ) ;
#15568 = LINE ( 'NONE', #7119, #14758 ) ;
#15569 = CARTESIAN_POINT ( 'NONE',  ( -13.37671366598624800, -20.91345986769124465, 5.053911344471881506 ) ) ;
#15570 = CARTESIAN_POINT ( 'NONE',  ( 6.340308582316796837, -22.36352608949544418, 4.520995438708343528 ) ) ;
#15571 = PLANE ( 'NONE',  #5316 ) ;
#15572 = ORIENTED_EDGE ( 'NONE', *, *, #17457, .F. ) ;
#15573 = ORIENTED_EDGE ( 'NONE', *, *, #19975, .F. ) ;
#15574 = CARTESIAN_POINT ( 'NONE',  ( 13.82120031190154208, 1.533115751011936867, 6.689942769197355865 ) ) ;
#15575 = CARTESIAN_POINT ( 'NONE',  ( -14.99999999999998401, -25.49999999999999645, 4.000000000000000000 ) ) ;
#15576 = ORIENTED_EDGE ( 'NONE', *, *, #18885, .T. ) ;
#15577 = EDGE_CURVE ( 'NONE', #17227, #19021, #6820, .T. ) ;
#15578 = DIRECTION ( 'NONE',  ( 0.000000000000000000, 1.000000000000000000, -0.000000000000000000 ) ) ;
#15579 = ORIENTED_EDGE ( 'NONE', *, *, #8886, .T. ) ;
#15580 = CARTESIAN_POINT ( 'NONE',  ( -0.1250000000000035805, 4.999999999999999112, 1.000000000000000000 ) ) ;
#15581 = CARTESIAN_POINT ( 'NONE',  ( 15.86404127825609400, 4.999999999999999112, 0.000000000000000000 ) ) ;
#15582 = DIRECTION ( 'NONE',  ( 0.000000000000000000, -1.000000000000000000, 0.000000000000000000 ) ) ;
#15583 = CARTESIAN_POINT ( 'NONE',  ( 1.720709671993384093, -9.114925383610804843, 1.622645897908254753 ) ) ;
#15584 = CARTESIAN_POINT ( 'NONE',  ( -9.305650798910056309, 4.999999999999999112, 1.000000000000000000 ) ) ;
#15585 = CARTESIAN_POINT ( 'NONE',  ( -13.09560260347216953, 4.265431475339161338, 5.020858537328734883 ) ) ;
#15586 = CARTESIAN_POINT ( 'NONE',  ( 7.746558582316794173, -21.94931252712234482, 5.250000000000000888 ) ) ;
#15587 = CARTESIAN_POINT ( 'NONE',  ( -12.62543384439201510, -20.97809085820452424, 4.782403934559678937 ) ) ;
#15588 = DIRECTION ( 'NONE',  ( 1.000000000000000000, 0.000000000000000000, 0.000000000000000000 ) ) ;
#15589 = CARTESIAN_POINT ( 'NONE',  ( 13.27780858231679595, -20.27099543870833642, 2.724438792969431589 ) ) ;
#15590 = CARTESIAN_POINT ( 'NONE',  ( 12.53469141768317741, -20.97900456129164581, 3.136473910504570917 ) ) ;
#15591 = CARTESIAN_POINT ( 'NONE',  ( -11.40969141768317918, -21.32581373872474373, 5.270995438708348857 ) ) ;
#15592 = ORIENTED_EDGE ( 'NONE', *, *, #7235, .T. ) ;
#15593 = CARTESIAN_POINT ( 'NONE',  ( 13.37499999999998224, -19.50000000000006040, 4.416666666666682062 ) ) ;
#15594 = VECTOR ( 'NONE', #9006, 1000.000000000000000 ) ;
#15595 = CARTESIAN_POINT ( 'NONE',  ( -1.819865260185086875, -9.122006307963404836, 1.624464420737683046 ) ) ;
#15596 = ORIENTED_EDGE ( 'NONE', *, *, #10058, .T. ) ;
#15597 = ORIENTED_EDGE ( 'NONE', *, *, #14082, .T. ) ;
#15598 = CARTESIAN_POINT ( 'NONE',  ( 25.54469207716615031, 0.000000000000000000, 0.000000000000000000 ) ) ;
#15599 = ADVANCED_FACE ( 'NONE', ( #3471, #6723, #13189, #18992, #1516, #17414, #19585, #10063 ), #17302, .T. ) ;
#15600 = CARTESIAN_POINT ( 'NONE',  ( -13.10012427866737639, 3.743776072700027324, 6.001983176248468332 ) ) ;
#15601 = CARTESIAN_POINT ( 'NONE',  ( -3.173374397671306912, -9.279487642487616483, 2.607523756204581211 ) ) ;
#15602 = CARTESIAN_POINT ( 'NONE',  ( -13.58606361274418184, -9.591287556442823714, 5.700679699621803209 ) ) ;
#15603 = EDGE_CURVE ( 'NONE', #11770, #15422, #6222, .T. ) ;
#15604 = DIRECTION ( 'NONE',  ( 0.000000000000000000, 1.000000000000000000, 0.000000000000000000 ) ) ;
#15605 = CARTESIAN_POINT ( 'NONE',  ( 6.183390479346035917, 9.000000000000001776, 1.000000000000000000 ) ) ;
#15606 = CARTESIAN_POINT ( 'NONE',  ( 13.12499999999999645, 5.000000000000047073, 3.999999999999996447 ) ) ;
#15607 = EDGE_CURVE ( 'NONE', #682, #3633, #5241, .T. ) ;
#15608 = DIRECTION ( 'NONE',  ( -0.000000000000000000, -0.000000000000000000, -1.000000000000000000 ) ) ;
#15609 = LINE ( 'NONE', #13623, #15645 ) ;
#15610 = CARTESIAN_POINT ( 'NONE',  ( -11.49655858231679595, -22.05068747287764452, 0.9999999999999978906 ) ) ;
#15611 = CARTESIAN_POINT ( 'NONE',  ( -2.762374231067749708, -9.968169115173667549, 1.841775933429679268 ) ) ;
#15612 = ORIENTED_EDGE ( 'NONE', *, *, #3626, .T. ) ;
#15613 = CARTESIAN_POINT ( 'NONE',  ( -13.37499999999998224, -20.24999999999991829, 4.333333333333343695 ) ) ;
#15614 = CARTESIAN_POINT ( 'NONE',  ( -26.19203811574920593, 0.000000000000000000, 1.000000000000000000 ) ) ;
#15615 = CARTESIAN_POINT ( 'NONE',  ( 5.871558582316795949, -19.49999999999998934, 3.449312527122348371 ) ) ;
#15616 = CARTESIAN_POINT ( 'NONE',  ( -4.097191417683177406, -22.46490103525075810, 4.479004561291653808 ) ) ;
#15617 = ORIENTED_EDGE ( 'NONE', *, *, #16394, .F. ) ;
#15618 = CARTESIAN_POINT ( 'NONE',  ( 13.87470602645761986, 4.985154336109792972, 4.916666666666650087 ) ) ;
#15619 = CARTESIAN_POINT ( 'NONE',  ( 12.62499999999998401, -20.24999999999998934, 2.439580858552613751 ) ) ;
#15620 = ORIENTED_EDGE ( 'NONE', *, *, #7708, .F. ) ;
#15621 = ORIENTED_EDGE ( 'NONE', *, *, #9559, .T. ) ;
#15622 = FACE_OUTER_BOUND ( 'NONE', #6378, .T. ) ;
#15623 = EDGE_LOOP ( 'NONE', ( #14921, #9149, #17584, #2668 ) ) ;
#15624 = CARTESIAN_POINT ( 'NONE',  ( -13.44218742460511073, -16.85703505742523234, 5.544429699623282914 ) ) ;
#15625 = EDGE_CURVE ( 'NONE', #16502, #351, #18006, .T. ) ;
#15626 = DIRECTION ( 'NONE',  ( 0.000000000000000000, 0.000000000000000000, 1.000000000000000000 ) ) ;
#15627 = AXIS2_PLACEMENT_3D ( 'NONE', #10009, #13452, #18171 ) ;
#15628 = ORIENTED_EDGE ( 'NONE', *, *, #5555, .F. ) ;
#15629 = FACE_OUTER_BOUND ( 'NONE', #15524, .T. ) ;
#15630 = VECTOR ( 'NONE', #18595, 1000.000000000000000 ) ;
#15631 = CARTESIAN_POINT ( 'NONE',  ( -13.12509927631103501, 5.009931486494128450, 3.999999999999983125 ) ) ;
#15632 = DIRECTION ( 'NONE',  ( 1.000000000000000000, 0.000000000000000000, 0.000000000000000000 ) ) ;
#15633 = CARTESIAN_POINT ( 'NONE',  ( 3.049989092406311109, -8.938202327316346896, 1.769874869409437279 ) ) ;
#15634 = LINE ( 'NONE', #20057, #6865 ) ;
#15635 = CARTESIAN_POINT ( 'NONE',  ( 13.12529397354238192, 5.014845663890295846, 3.000000000000000000 ) ) ;
#15636 = DIRECTION ( 'NONE',  ( 1.000000000000000000, 0.000000000000000000, 0.000000000000000000 ) ) ;
#15637 = CARTESIAN_POINT ( 'NONE',  ( 4.247260319564023945, 4.999999999999999112, 0.000000000000000000 ) ) ;
#15638 = DIRECTION ( 'NONE',  ( 1.000000000000000000, 0.000000000000000000, 0.000000000000000000 ) ) ;
#15639 = AXIS2_PLACEMENT_3D ( 'NONE', #12829, #6154, #15861 ) ;
#15640 = CARTESIAN_POINT ( 'NONE',  ( 6.347191417683176518, -21.53509896474923835, 2.520995438708346192 ) ) ;
#15641 = CARTESIAN_POINT ( 'NONE',  ( -12.62499999999998401, -19.49999999999998934, 2.439580858552613751 ) ) ;
#15642 = EDGE_CURVE ( 'NONE', #7438, #18614, #701, .T. ) ;
#15643 = CARTESIAN_POINT ( 'NONE',  ( -8.215308582316795949, -23.02099543870833998, 3.136473910504556262 ) ) ;
#15644 = CARTESIAN_POINT ( 'NONE',  ( -5.690941417683177406, -23.80360840875937001, 5.231925497173365081 ) ) ;
#15645 = VECTOR ( 'NONE', #20031, 1000.000000000000000 ) ;
#15646 = ORIENTED_EDGE ( 'NONE', *, *, #10564, .F. ) ;
#15647 = CARTESIAN_POINT ( 'NONE',  ( 13.37732542738919328, -19.38256591684242025, 4.710253041318374301 ) ) ;
#15648 = CARTESIAN_POINT ( 'NONE',  ( 9.000000000000000000, -9.999999999999991118, 1.000000000000000000 ) ) ;
#15649 = ORIENTED_EDGE ( 'NONE', *, *, #12824, .T. ) ;
#15650 = AXIS2_PLACEMENT_3D ( 'NONE', #14390, #6460, #12823 ) ;
#15651 = DIRECTION ( 'NONE',  ( 0.000000000000000000, -1.000000000000000000, 0.000000000000000000 ) ) ;
#15652 = VERTEX_POINT ( 'NONE', #12497 ) ;
#15653 = CARTESIAN_POINT ( 'NONE',  ( 1.717920576997000737, -9.114924032904250240, 2.372645551019823884 ) ) ;
#15654 = EDGE_CURVE ( 'NONE', #10445, #6014, #18893, .T. ) ;
#15655 = EDGE_CURVE ( 'NONE', #8351, #2127, #12522, .T. ) ;
#15656 = VECTOR ( 'NONE', #5403, 1000.000000000000000 ) ;
#15657 = VECTOR ( 'NONE', #390, 1000.000000000000000 ) ;
#15658 = ORIENTED_EDGE ( 'NONE', *, *, #5438, .T. ) ;
#15659 = LINE ( 'NONE', #18709, #15991 ) ;
#15660 = CARTESIAN_POINT ( 'NONE',  ( 0.000000000000000000, 10.00000000000000000, 1.000000000000000000 ) ) ;
#15661 = VECTOR ( 'NONE', #15744, 1000.000000000000000 ) ;
#15662 = CARTESIAN_POINT ( 'NONE',  ( -2.742252025265078608, -15.06657917462210605, 2.958534504914692942 ) ) ;
#15663 = FACE_OUTER_BOUND ( 'NONE', #11945, .T. ) ;
#15664 = LINE ( 'NONE', #4379, #6023 ) ;
#15665 = CARTESIAN_POINT ( 'NONE',  ( 12.62844141768317741, -20.24999999999999289, 3.550687472877664952 ) ) ;
#15666 = PLANE ( 'NONE',  #5524 ) ;
#15667 = ADVANCED_FACE ( 'NONE', ( #13596 ), #19899, .T. ) ;
#15668 = CARTESIAN_POINT ( 'NONE',  ( -7.190941417683176518, -23.27327832286946219, 4.701595411283453707 ) ) ;
#15669 = VERTEX_POINT ( 'NONE', #15174 ) ;
#15670 = CARTESIAN_POINT ( 'NONE',  ( 6.246558582316794173, -21.94931252712234482, 5.250000000000000888 ) ) ;
#15671 = LINE ( 'NONE', #6370, #2392 ) ;
#15672 = CARTESIAN_POINT ( 'NONE',  ( -12.66863463945108137, -18.79645070772368953, 6.267287912489321045 ) ) ;
#15673 = AXIS2_PLACEMENT_3D ( 'NONE', #2786, #17305, #9162 ) ;
#15674 = VECTOR ( 'NONE', #7182, 1000.000000000000000 ) ;
#15675 = CARTESIAN_POINT ( 'NONE',  ( 9.434058582316794173, -23.20159541128345992, 4.773278322869455970 ) ) ;
#15676 = DIRECTION ( 'NONE',  ( -1.000000000000000000, 3.469446951953619119E-16, 0.000000000000000000 ) ) ;
#15677 = AXIS2_PLACEMENT_3D ( 'NONE', #8871, #4059, #3749 ) ;
#15678 = ORIENTED_EDGE ( 'NONE', *, *, #14394, .T. ) ;
#15679 = CARTESIAN_POINT ( 'NONE',  ( 13.43273460392801155, -18.08440250163749496, 6.268067769197452677 ) ) ;
#15680 = CARTESIAN_POINT ( 'NONE',  ( 23.60856191738414012, 4.999999999999999112, 1.000000000000000000 ) ) ;
#15681 =( NAMED_UNIT ( * ) PLANE_ANGLE_UNIT ( ) SI_UNIT ( $, .RADIAN. ) );
#15682 = ORIENTED_EDGE ( 'NONE', *, *, #18479, .T. ) ;
#15683 = LINE ( 'NONE', #1669, #17807 ) ;
#15684 = EDGE_CURVE ( 'NONE', #4496, #351, #11865, .T. ) ;
#15685 = ORIENTED_EDGE ( 'NONE', *, *, #7678, .F. ) ;
#15686 = CARTESIAN_POINT ( 'NONE',  ( -9.340308582316794173, -22.67418626127525982, 5.270995438708342640 ) ) ;
#15687 = DIRECTION ( 'NONE',  ( 0.000000000000000000, -0.000000000000000000, 1.000000000000000000 ) ) ;
#15688 = DIRECTION ( 'NONE',  ( 1.000000000000000000, 0.000000000000000000, 0.000000000000000000 ) ) ;
#15689 = CARTESIAN_POINT ( 'NONE',  ( 1.513434189748285918, -8.364917468222230923, 1.622643865078341907 ) ) ;
#15690 = CIRCLE ( 'NONE', #8004, 10.00000000000000000 ) ;
#15691 = CARTESIAN_POINT ( 'NONE',  ( -2.187849085826861550, 10.00000000000000000, 1.000000000000000000 ) ) ;
#15692 = CARTESIAN_POINT ( 'NONE',  ( -13.08799567112409790, 3.881281391764801025, 5.254907606674271037 ) ) ;
#15693 = CARTESIAN_POINT ( 'NONE',  ( 7.090308582316794173, -21.32581373872472597, 1.729004561291657582 ) ) ;
#15694 = CARTESIAN_POINT ( 'NONE',  ( -13.89075858682503650, 5.045808634669852744, 6.406973581600956535 ) ) ;
#15695 = EDGE_CURVE ( 'NONE', #10100, #9451, #2306, .T. ) ;
#15696 = VECTOR ( 'NONE', #6275, 1000.000000000000000 ) ;
#15697 = CARTESIAN_POINT ( 'NONE',  ( 9.246558582316794173, -21.94931252712234482, 5.250000000000000888 ) ) ;
#15698 = CARTESIAN_POINT ( 'NONE',  ( 12.90280858231679595, -22.46490103525074034, 2.520995438708341307 ) ) ;
#15699 = CARTESIAN_POINT ( 'NONE',  ( -12.44094141768317741, -20.72672167713052715, 2.298404588716546293 ) ) ;
#15700 = ORIENTED_EDGE ( 'NONE', *, *, #10950, .T. ) ;
#15701 = CARTESIAN_POINT ( 'NONE',  ( 13.42766088059286922, -16.84062553004338625, 4.794749963382423985 ) ) ;
#15702 = CARTESIAN_POINT ( 'NONE',  ( -2.786182376113650605, -10.12667130264514626, 1.882483419865550900 ) ) ;
#15703 = VERTEX_POINT ( 'NONE', #2513 ) ;
#15704 = UNCERTAINTY_MEASURE_WITH_UNIT (LENGTH_MEASURE( 1.000000000000000082E-05 ), #11919, 'distance_accuracy_value', 'NONE');
#15705 = VERTEX_POINT ( 'NONE', #19800 ) ;
#15706 = PLANE ( 'NONE',  #16457 ) ;
#15707 = PRODUCT_RELATED_PRODUCT_CATEGORY ( 'part', '', ( #1665 ) ) ;
#15708 = CIRCLE ( 'NONE', #12036, 0.3750000000000003331 ) ;
#15709 = CARTESIAN_POINT ( 'NONE',  ( -12.68288333306630378, -17.32689168014509207, 5.548858176248425700 ) ) ;
#15710 = CARTESIAN_POINT ( 'NONE',  ( -1.126276606324276619, -8.364917468222230923, 2.372643865078341019 ) ) ;
#15711 = CARTESIAN_POINT ( 'NONE',  ( -13.40382044110196347, -18.79456772435387890, 5.502763032956559108 ) ) ;
#15712 = DIRECTION ( 'NONE',  ( 0.1736481776669292765, -0.9848077530122082424, 0.000000000000000000 ) ) ;
#15713 = CARTESIAN_POINT ( 'NONE',  ( 0.000000000000000000, 9.000000000000001776, 1.000000000000000000 ) ) ;
#15714 = CARTESIAN_POINT ( 'NONE',  ( 11.02780858231679595, -23.72900456129165292, 4.275561207030568411 ) ) ;
#15715 = DIRECTION ( 'NONE',  ( 1.000000000000000000, 6.938893903907222067E-15, 0.000000000000000000 ) ) ;
#15716 = CARTESIAN_POINT ( 'NONE',  ( 13.10026320386584153, 3.000791795219782454, 6.736037912489353019 ) ) ;
#15717 = CARTESIAN_POINT ( 'NONE',  ( -6.527808582316795949, -24.47900456129166358, 4.586221378810390270 ) ) ;
#15718 = CARTESIAN_POINT ( 'NONE',  ( -2.088806020750596737, -10.42712783963456857, 1.767030719737609168 ) ) ;
#15719 = ORIENTED_EDGE ( 'NONE', *, *, #11605, .T. ) ;
#15720 = AXIS2_PLACEMENT_3D ( 'NONE', #15489, #2423, #13708 ) ;
#15721 = CARTESIAN_POINT ( 'NONE',  ( -13.37503071710846925, -20.24844878602346299, 4.564052989354591361 ) ) ;
#15722 = LINE ( 'NONE', #16877, #695 ) ;
#15723 = VECTOR ( 'NONE', #13525, 1000.000000000000000 ) ;
#15724 = EDGE_CURVE ( 'NONE', #16371, #3612, #11827, .T. ) ;
#15725 = CARTESIAN_POINT ( 'NONE',  ( 6.902808582316795949, -23.08622137881038938, 1.020995438708339309 ) ) ;
#15726 = CARTESIAN_POINT ( 'NONE',  ( -6.159691417683175629, -22.36352608949543352, 2.479004561291652031 ) ) ;
#15727 = VERTEX_POINT ( 'NONE', #8697 ) ;
#15728 = VECTOR ( 'NONE', #13704, 1000.000000000000000 ) ;
#15729 = CARTESIAN_POINT ( 'NONE',  ( 13.42074492158312715, -18.68988146005270679, 6.255046935864005064 ) ) ;
#15730 = DIRECTION ( 'NONE',  ( -0.000000000000000000, -0.000000000000000000, -1.000000000000000000 ) ) ;
#15731 = PLANE ( 'NONE',  #11013 ) ;
#15732 = ORIENTED_EDGE ( 'NONE', *, *, #2066, .T. ) ;
#15733 = ORIENTED_EDGE ( 'NONE', *, *, #11710, .F. ) ;
#15734 = CARTESIAN_POINT ( 'NONE',  ( -13.84504075139246915, 3.487057945321567765, 5.981929699623240282 ) ) ;
#15735 = DIRECTION ( 'NONE',  ( 0.000000000000000000, -0.8660254037844363761, 0.5000000000000041078 ) ) ;
#15736 = EDGE_LOOP ( 'NONE', ( #6217, #11759, #16423, #5468 ) ) ;
#15737 = CARTESIAN_POINT ( 'NONE',  ( -15.61404127825609223, 4.999999999999999112, 1.000000000000000000 ) ) ;
#15738 = CARTESIAN_POINT ( 'NONE',  ( 2.436080212393455735, -9.483920418190111334, 2.467411194204634839 ) ) ;
#15739 = AXIS2_PLACEMENT_3D ( 'NONE', #7261, #17082, #4219 ) ;
#15740 = CARTESIAN_POINT ( 'NONE',  ( -13.50000000000000178, 0.000000000000000000, 2.000000000000000000 ) ) ;
#15741 = CARTESIAN_POINT ( 'NONE',  ( 1.619022621591187150, -9.114917468222230923, 1.622643865078341463 ) ) ;
#15742 = CARTESIAN_POINT ( 'NONE',  ( 15.06494360078803041, 11.64110105645932691, 10.00000000000000000 ) ) ;
#15743 = CARTESIAN_POINT ( 'NONE',  ( -4.250698171653726654, 10.00000000000000000, 0.000000000000000000 ) ) ;
#15744 = DIRECTION ( 'NONE',  ( -1.000000000000000000, 0.000000000000000000, 0.000000000000000000 ) ) ;
#15745 = DIRECTION ( 'NONE',  ( 1.192622389734054384E-16, -1.000000000000000000, 0.000000000000000000 ) ) ;
#15746 = CARTESIAN_POINT ( 'NONE',  ( -12.66615398568989370, -20.44683554016566163, 3.545542780064843136 ) ) ;
#15747 = CARTESIAN_POINT ( 'NONE',  ( 6.722191417683176518, -21.02099543870834353, 3.964901035250761208 ) ) ;
#15748 = CARTESIAN_POINT ( 'NONE',  ( -13.12529397354238192, 5.014845663890295846, 3.000000000000000000 ) ) ;
#15749 = CARTESIAN_POINT ( 'NONE',  ( -11.96530858231679773, -20.97900456129165647, 3.863526089495444626 ) ) ;
#15750 = EDGE_CURVE ( 'NONE', #7608, #11568, #10163, .T. ) ;
#15751 = CARTESIAN_POINT ( 'NONE',  ( -11.40969141768318096, -21.32581373872474373, 5.270995438708348857 ) ) ;
#15752 = ORIENTED_EDGE ( 'NONE', *, *, #16816, .T. ) ;
#15753 = CARTESIAN_POINT ( 'NONE',  ( 13.37503747255156306, -19.49810763614315690, 4.531249681074674740 ) ) ;
#15754 = DIRECTION ( 'NONE',  ( -1.000000000000000000, 0.000000000000000000, 0.000000000000000000 ) ) ;
#15755 = ORIENTED_EDGE ( 'NONE', *, *, #16617, .T. ) ;
#15756 = VECTOR ( 'NONE', #19143, 1000.000000000000000 ) ;
#15757 = DIRECTION ( 'NONE',  ( 0.000000000000000000, -0.000000000000000000, 1.000000000000000000 ) ) ;
#15758 = ORIENTED_EDGE ( 'NONE', *, *, #9122, .T. ) ;
#15759 = CARTESIAN_POINT ( 'NONE',  ( 1.772926875221950249, -9.883376166076789815, 2.377384427436886494 ) ) ;
#15760 = EDGE_CURVE ( 'NONE', #9416, #9078, #950, .T. ) ;
#15761 = EDGE_CURVE ( 'NONE', #8747, #18643, #13865, .T. ) ;
#15762 = ORIENTED_EDGE ( 'NONE', *, *, #14634, .F. ) ;
#15763 = CARTESIAN_POINT ( 'NONE',  ( 7.940941417683176518, -20.72672167713052715, 2.298404588716546293 ) ) ;
#15764 = PLANE ( 'NONE',  #3968 ) ;
#15765 = CARTESIAN_POINT ( 'NONE',  ( -2.110348196723525138, -10.58007678474401914, 1.806311064303893099 ) ) ;
#15766 = FACE_OUTER_BOUND ( 'NONE', #1333, .T. ) ;
#15767 = CARTESIAN_POINT ( 'NONE',  ( -20.92243175760212637, 0.000000000000000000, 1.000000000000000000 ) ) ;
#15768 = VECTOR ( 'NONE', #5074, 1000.000000000000000 ) ;
#15769 = CARTESIAN_POINT ( 'NONE',  ( 13.50000000000000178, 7.806255641895631925E-15, 1.000000000000000000 ) ) ;
#15770 = CARTESIAN_POINT ( 'NONE',  ( 6.347191417683176518, -20.91377862118959285, 1.020995438708345082 ) ) ;
#15771 = LINE ( 'NONE', #17546, #16221 ) ;
#15772 = CARTESIAN_POINT ( 'NONE',  ( -10.28469141768318096, -23.77099543870834353, 4.174186261275252718 ) ) ;
#15773 = ADVANCED_FACE ( 'NONE', ( #7136 ), #14959, .T. ) ;
#15774 = ORIENTED_EDGE ( 'NONE', *, *, #2217, .F. ) ;
#15775 = CARTESIAN_POINT ( 'NONE',  ( 13.09030858231679417, -21.01515356694490322, 0.9790045612916562501 ) ) ;
#15776 = DIRECTION ( 'NONE',  ( 0.000000000000000000, 1.000000000000000000, 0.000000000000000000 ) ) ;
#15777 = CARTESIAN_POINT ( 'NONE',  ( -12.62927505847832776, -20.78410954684871825, 5.373974324164845662 ) ) ;
#15778 = ORIENTED_EDGE ( 'NONE', *, *, #8695, .F. ) ;
#15779 = AXIS2_PLACEMENT_3D ( 'NONE', #2979, #12973, #14442 ) ;
#15780 = CARTESIAN_POINT ( 'NONE',  ( 9.527808582316792396, -23.72900456129165647, 4.275561207030568411 ) ) ;
#15781 = LINE ( 'NONE', #7433, #20367 ) ;
#15782 = ORIENTED_EDGE ( 'NONE', *, *, #3778, .F. ) ;
#15783 = CARTESIAN_POINT ( 'NONE',  ( -0.000000000000000000, 11.64110105645932691, 0.000000000000000000 ) ) ;
#15784 = FILL_AREA_STYLE_COLOUR ( '', #6355 ) ;
#15785 = EDGE_LOOP ( 'NONE', ( #1746, #7715, #3852, #7351 ) ) ;
#15786 = VECTOR ( 'NONE', #4522, 1000.000000000000000 ) ;
#15787 = DIRECTION ( 'NONE',  ( 1.000000000000000000, 1.734723475976787570E-15, 0.000000000000000000 ) ) ;
#15788 = EDGE_LOOP ( 'NONE', ( #11030, #15430, #11920, #8221 ) ) ;
#15789 = CARTESIAN_POINT ( 'NONE',  ( -6.340308582316793284, -22.67418626127525982, 5.270995438708342640 ) ) ;
#15790 = DIRECTION ( 'NONE',  ( -0.000000000000000000, -1.000000000000000000, 0.000000000000000000 ) ) ;
#15791 = CARTESIAN_POINT ( 'NONE',  ( 13.15332036705482466, 5.722234611034569873, 3.999999999999985345 ) ) ;
#15792 = CARTESIAN_POINT ( 'NONE',  ( 0.2815691515810352930, -9.114917468222230923, 1.622643865078524206 ) ) ;
#15793 = DIRECTION ( 'NONE',  ( 1.000000000000000000, 0.000000000000000000, 0.000000000000000000 ) ) ;
#15794 = CARTESIAN_POINT ( 'NONE',  ( -13.38929389708972195, -18.77815819697223887, 4.753083296715700179 ) ) ;
#15795 = CARTESIAN_POINT ( 'NONE',  ( 4.840308582316793284, -22.67418626127525982, 5.270995438708342640 ) ) ;
#15796 = CARTESIAN_POINT ( 'NONE',  ( -13.90326467458556969, 5.677366066573198644, 5.457668599364335904 ) ) ;
#15797 = AXIS2_PLACEMENT_3D ( 'NONE', #3980, #10363, #7332 ) ;
#15798 = ADVANCED_FACE ( 'NONE', ( #11927 ), #18321, .F. ) ;
#15799 = EDGE_CURVE ( 'NONE', #18810, #8332, #5349, .T. ) ;
#15800 = CARTESIAN_POINT ( 'NONE',  ( 3.944195004867015353, -21.66042601004066981, 5.025996387692261536 ) ) ;
#15801 = CARTESIAN_POINT ( 'NONE',  ( -20.49999999999998224, -21.99999999999999645, 12.00000000000000355 ) ) ;
#15802 = CARTESIAN_POINT ( 'NONE',  ( 4.378441417683176518, -22.99999999999999645, 3.449312527122335048 ) ) ;
#15803 = CARTESIAN_POINT ( 'NONE',  ( -5.309058582316794173, -23.27327832286945153, 2.298404588716537411 ) ) ;
#15804 = ORIENTED_EDGE ( 'NONE', *, *, #12299, .T. ) ;
#15805 = ADVANCED_FACE ( 'NONE', ( #10477 ), #16532, .T. ) ;
#15806 = CARTESIAN_POINT ( 'NONE',  ( 13.37847682517167947, -19.32442032882675775, 4.733786629989340078 ) ) ;
#15807 = CARTESIAN_POINT ( 'NONE',  ( -1.619022621591187150, -9.114917468222230923, 1.622643865078341463 ) ) ;
#15808 = ORIENTED_EDGE ( 'NONE', *, *, #6279, .F. ) ;
#15809 = ORIENTED_EDGE ( 'NONE', *, *, #10567, .F. ) ;
#15810 = CARTESIAN_POINT ( 'NONE',  ( -27.49999999999999645, -4.770489558936219510E-14, 1.000000000000000000 ) ) ;
#15811 = EDGE_CURVE ( 'NONE', #20271, #16070, #2110, .T. ) ;
#15812 = CARTESIAN_POINT ( 'NONE',  ( -14.49999999999999645, -21.00000000000000355, 4.000000000000000000 ) ) ;
#15813 = CARTESIAN_POINT ( 'NONE',  ( 0.000000000000000000, -8.364917468222230923, 2.372643865078341019 ) ) ;
#15814 = DIRECTION ( 'NONE',  ( 1.000000000000000000, 0.000000000000000000, 0.000000000000000000 ) ) ;
#15815 = DIRECTION ( 'NONE',  ( 0.000000000000000000, 0.000000000000000000, -1.000000000000000000 ) ) ;
#15816 = CARTESIAN_POINT ( 'NONE',  ( 4.750698171653723989, 0.000000000000000000, 1.000000000000000000 ) ) ;
#15817 = CARTESIAN_POINT ( 'NONE',  ( 9.902808582316794173, -22.77556120703056308, 1.770995438708340197 ) ) ;
#15818 = LINE ( 'NONE', #10915, #15409 ) ;
#15819 = CARTESIAN_POINT ( 'NONE',  ( 13.10745701327265778, 3.364079170269163921, 6.743850412489304169 ) ) ;
#15820 = CARTESIAN_POINT ( 'NONE',  ( -5.215308582316795949, -24.52099543870834708, 2.515153566944913432 ) ) ;
#15821 = CARTESIAN_POINT ( 'NONE',  ( -1.700193846275138032, -9.865151716929458914, 2.372704024825938340 ) ) ;
#15822 = AXIS2_PLACEMENT_3D ( 'NONE', #20524, #6177, #7444 ) ;
#15823 = VERTEX_POINT ( 'NONE', #850 ) ;
#15824 = CARTESIAN_POINT ( 'NONE',  ( -13.83051420738022763, 3.503467472703414742, 5.232249963382380464 ) ) ;
#15825 = CARTESIAN_POINT ( 'NONE',  ( 0.000000000000000000, 0.000000000000000000, 1.000000000000000000 ) ) ;
#15826 = CARTESIAN_POINT ( 'NONE',  ( 7.565941417683177406, -23.73192549717336064, 1.696391591240623331 ) ) ;
#15827 = CARTESIAN_POINT ( 'NONE',  ( -11.02780858231679595, -22.97900456129165647, 3.964901035250747885 ) ) ;
#15828 = EDGE_LOOP ( 'NONE', ( #7895, #4955, #12231, #576 ) ) ;
#15829 = CARTESIAN_POINT ( 'NONE',  ( 13.44712222274167246, -17.35782775154002522, 6.283692769197384287 ) ) ;
#15830 = CARTESIAN_POINT ( 'NONE',  ( 12.63943061533661982, -19.52125392549825733, 5.470334935344855154 ) ) ;
#15831 = CARTESIAN_POINT ( 'NONE',  ( 17.11324865405191176, -10.99999999999999645, 2.000000000000000000 ) ) ;
#15832 = EDGE_LOOP ( 'NONE', ( #177, #20435, #9226, #633 ) ) ;
#15833 = ORIENTED_EDGE ( 'NONE', *, *, #3105, .F. ) ;
#15834 = CARTESIAN_POINT ( 'NONE',  ( 4.315753587183822404, -21.47141115243053378, 5.558207674221720573 ) ) ;
#15835 = ADVANCED_FACE ( 'NONE', ( #7232 ), #19998, .T. ) ;
#15836 = DIRECTION ( 'NONE',  ( 0.000000000000000000, 1.000000000000000000, -0.000000000000000000 ) ) ;
#15837 = ORIENTED_EDGE ( 'NONE', *, *, #12582, .T. ) ;
#15838 = DIRECTION ( 'NONE',  ( 1.000000000000000000, 0.000000000000000000, 0.000000000000000000 ) ) ;
#15839 = CARTESIAN_POINT ( 'NONE',  ( 2.875042468481914248, -11.91375063635796039, 3.091440134965714126 ) ) ;
#15840 = LINE ( 'NONE', #19104, #16664 ) ;
#15841 = CARTESIAN_POINT ( 'NONE',  ( 3.436477319925839602, -9.631595465688135960, 1.947952079262935676 ) ) ;
#15842 = CARTESIAN_POINT ( 'NONE',  ( -24.79469207716615031, 9.000000000000001776, 0.000000000000000000 ) ) ;
#15843 = DIRECTION ( 'NONE',  ( 1.000000000000000000, 0.000000000000000000, 0.000000000000000000 ) ) ;
#15844 = DIRECTION ( 'NONE',  ( 1.000000000000000000, -0.000000000000000000, -0.000000000000000000 ) ) ;
#15845 = CARTESIAN_POINT ( 'NONE',  ( 10.49999999999999467, -9.999999999999991118, 2.000000000000000000 ) ) ;
#15846 = CARTESIAN_POINT ( 'NONE',  ( -12.80905858231679417, -23.27327832286945153, 2.298404588716537411 ) ) ;
#15847 = PRODUCT_DEFINITION_SHAPE ( 'NONE', 'NONE',  #12257 ) ;
#15848 = CARTESIAN_POINT ( 'NONE',  ( 9.065941417683177406, -22.67126532539353789, 2.757051763020445634 ) ) ;
#15849 = CARTESIAN_POINT ( 'NONE',  ( -13.12529397354238192, 5.014845663890295846, 4.666666666666619889 ) ) ;
#15850 = CARTESIAN_POINT ( 'NONE',  ( -12.99655858231679417, -22.05068747287764452, 1.749999999999998446 ) ) ;
#15851 = CARTESIAN_POINT ( 'NONE',  ( -4.378441417683176518, -24.50000000000000000, 3.449312527122335048 ) ) ;
#15852 = ORIENTED_EDGE ( 'NONE', *, *, #4137, .F. ) ;
#15853 = CARTESIAN_POINT ( 'NONE',  ( 13.09073190589589331, 4.019461247742575516, 5.257453802652931607 ) ) ;
#15854 = CARTESIAN_POINT ( 'NONE',  ( -22.81633994409548549, 11.64110105645932691, 10.00000000000000000 ) ) ;
#15855 = EDGE_LOOP ( 'NONE', ( #17716, #3487, #14692, #13796 ) ) ;
#15856 = LINE ( 'NONE', #1535, #18679 ) ;
#15857 = VERTEX_POINT ( 'NONE', #5769 ) ;
#15858 = PLANE ( 'NONE',  #7091 ) ;
#15859 = ORIENTED_EDGE ( 'NONE', *, *, #15862, .T. ) ;
#15860 = LINE ( 'NONE', #17537, #14662 ) ;
#15861 = DIRECTION ( 'NONE',  ( -0.9908228861781570584, 0.1309180808328758994, -0.03362237850931586169 ) ) ;
#15862 = EDGE_CURVE ( 'NONE', #2296, #17379, #8493, .T. ) ;
#15863 = VECTOR ( 'NONE', #13600, 1000.000000000000000 ) ;
#15864 = VECTOR ( 'NONE', #8283, 1000.000000000000000 ) ;
#15865 = CARTESIAN_POINT ( 'NONE',  ( -1.619022621591187150, -9.114917468222230923, 2.372643865078341019 ) ) ;
#15866 = DIRECTION ( 'NONE',  ( -0.000000000000000000, -0.000000000000000000, -1.000000000000000000 ) ) ;
#15867 = CARTESIAN_POINT ( 'NONE',  ( -12.24655858231679240, -21.94931252712234482, 5.250000000000000888 ) ) ;
#15868 = ADVANCED_FACE ( 'NONE', ( #11727 ), #19686, .T. ) ;
#15869 = EDGE_CURVE ( 'NONE', #16909, #381, #17159, .T. ) ;
#15870 = CARTESIAN_POINT ( 'NONE',  ( 6.253441417683175629, -21.94931252712233061, 0.9999999999999978906 ) ) ;
#15871 = FACE_OUTER_BOUND ( 'NONE', #20140, .T. ) ;
#15872 = CARTESIAN_POINT ( 'NONE',  ( -8.315941417683177406, -20.79840458871654363, 4.773278322869464851 ) ) ;
#15873 = VECTOR ( 'NONE', #8114, 1000.000000000000000 ) ;
#15874 = ORIENTED_EDGE ( 'NONE', *, *, #8029, .F. ) ;
#15875 = CARTESIAN_POINT ( 'NONE',  ( 6.715308582316794173, -23.77099543870833998, 2.825813738724734847 ) ) ;
#15876 = CARTESIAN_POINT ( 'NONE',  ( 10.00000000000000533, -30.00000000000000355, 0.000000000000000000 ) ) ;
#15877 = CARTESIAN_POINT ( 'NONE',  ( -12.96597876160390683, -3.780572539034193102, 6.590204579154564257 ) ) ;
#15878 = CARTESIAN_POINT ( 'NONE',  ( 5.590308582316794173, -21.32581373872472597, 1.729004561291657582 ) ) ;
#15879 = LINE ( 'NONE', #3439, #10337 ) ;
#15880 = ORIENTED_EDGE ( 'NONE', *, *, #19670, .F. ) ;
#15881 = DIRECTION ( 'NONE',  ( 0.000000000000000000, 1.000000000000000000, -0.000000000000000000 ) ) ;
#15882 = AXIS2_PLACEMENT_3D ( 'NONE', #12527, #9594, #12626 ) ;
#15883 = VERTEX_POINT ( 'NONE', #17054 ) ;
#15884 = DIRECTION ( 'NONE',  ( -0.000000000000000000, -0.000000000000000000, -1.000000000000000000 ) ) ;
#15885 = EDGE_LOOP ( 'NONE', ( #20413, #10558, #3608, #12748 ) ) ;
#15886 = CARTESIAN_POINT ( 'NONE',  ( -12.52780858231679773, -24.47900456129166358, 4.586221378810390270 ) ) ;
#15887 = CARTESIAN_POINT ( 'NONE',  ( 12.62888984277510218, -20.05356293986039873, 5.111704976569332537 ) ) ;
#15888 = ADVANCED_FACE ( 'NONE', ( #3044 ), #2733, .T. ) ;
#15889 = CARTESIAN_POINT ( 'NONE',  ( -14.99999999999998046, -26.49999999999999645, 1.000000000000000000 ) ) ;
#15890 = CARTESIAN_POINT ( 'NONE',  ( 2.340131407102140848, -12.21153219924485889, 2.225301406344140531 ) ) ;
#15891 = CARTESIAN_POINT ( 'NONE',  ( 15.50000000000000178, -20.99999999999999645, 4.000000000000000000 ) ) ;
#15892 = CARTESIAN_POINT ( 'NONE',  ( -13.84485691484488257, 4.227774199669918964, 5.063753864839139140 ) ) ;
#15893 = CARTESIAN_POINT ( 'NONE',  ( 9.434058582316794173, -23.20159541128345992, 4.773278322869455970 ) ) ;
#15894 = CARTESIAN_POINT ( 'NONE',  ( -13.90439735423812273, 5.734566389025032684, 4.791666666666684726 ) ) ;
#15895 = DIRECTION ( 'NONE',  ( 1.000000000000000000, 0.000000000000000000, 0.000000000000000000 ) ) ;
#15896 = CARTESIAN_POINT ( 'NONE',  ( -10.09030858231679595, -21.01515356694490322, 0.9790045612916562501 ) ) ;
#15897 = DIRECTION ( 'NONE',  ( 0.000000000000000000, -0.000000000000000000, 1.000000000000000000 ) ) ;
#15898 = EDGE_CURVE ( 'NONE', #2944, #14584, #9008, .T. ) ;
#15899 = CARTESIAN_POINT ( 'NONE',  ( 7.472191417683177406, -22.97900456129165292, 3.035098964749240125 ) ) ;
#15900 = CARTESIAN_POINT ( 'NONE',  ( -10.09719141768317563, -22.77556120703057729, 5.229004561291656472 ) ) ;
#15901 = ORIENTED_EDGE ( 'NONE', *, *, #11829, .T. ) ;
#15902 = CARTESIAN_POINT ( 'NONE',  ( 13.83973345681288158, 3.969039569021246550, 5.242263935944164288 ) ) ;
#15903 = DIRECTION ( 'NONE',  ( 0.000000000000000000, 0.000000000000000000, 1.000000000000000000 ) ) ;
#15904 = ORIENTED_EDGE ( 'NONE', *, *, #10655, .F. ) ;
#15905 = PRODUCT_DEFINITION_CONTEXT ( 'detailed design', #6151, 'design' ) ;
#15906 = ORIENTED_EDGE ( 'NONE', *, *, #2779, .T. ) ;
#15907 = CIRCLE ( 'NONE', #6897, 10.00000000000000000 ) ;
#15908 = CARTESIAN_POINT ( 'NONE',  ( -2.187849085826861550, 0.000000000000000000, 1.000000000000000000 ) ) ;
#15909 = FACE_OUTER_BOUND ( 'NONE', #5805, .T. ) ;
#15910 = ADVANCED_FACE ( 'NONE', ( #12450 ), #12239, .T. ) ;
#15911 = EDGE_CURVE ( 'NONE', #15088, #6051, #17252, .T. ) ;
#15912 = CARTESIAN_POINT ( 'NONE',  ( -3.594802210173583035, -11.77224174634763898, 3.247712807842289884 ) ) ;
#15913 = CYLINDRICAL_SURFACE ( 'NONE', #16359, 10.00000000000000000 ) ;
#15914 = DIRECTION ( 'NONE',  ( 1.000000000000000000, 0.000000000000000000, 0.000000000000000000 ) ) ;
#15915 = CARTESIAN_POINT ( 'NONE',  ( -12.62888984277510218, -20.05356293986039873, 5.111704976569332537 ) ) ;
#15916 = CARTESIAN_POINT ( 'NONE',  ( 12.90280858231679595, -22.77556120703056308, 1.770995438708340197 ) ) ;
#15917 = DIRECTION ( 'NONE',  ( 0.000000000000000000, 0.000000000000000000, 1.000000000000000000 ) ) ;
#15918 = CARTESIAN_POINT ( 'NONE',  ( 13.11824772738305356, 3.909010232842670796, 6.755569162489314827 ) ) ;
#15919 = CARTESIAN_POINT ( 'NONE',  ( -1.882415164465650825, -10.11790622164856224, 2.437616430916333510 ) ) ;
#15920 = ORIENTED_EDGE ( 'NONE', *, *, #10110, .T. ) ;
#15921 = AXIS2_PLACEMENT_3D ( 'NONE', #11849, #11747, #18140 ) ;
#15922 = CARTESIAN_POINT ( 'NONE',  ( -13.84264281492353987, 3.365962153638767607, 5.979325532956542233 ) ) ;
#15923 = LINE ( 'NONE', #3274, #11380 ) ;
#15924 = ADVANCED_FACE ( 'NONE', ( #1469 ), #10989, .T. ) ;
#15925 = CARTESIAN_POINT ( 'NONE',  ( 8.222191417683175629, -19.52099543870834353, 4.586221378810406257 ) ) ;
#15926 = CARTESIAN_POINT ( 'NONE',  ( -5.503441417683177406, -22.05068747287766229, 4.499999999999999112 ) ) ;
#15927 = ORIENTED_EDGE ( 'NONE', *, *, #4442, .F. ) ;
#15928 = CARTESIAN_POINT ( 'NONE',  ( 13.48548920624593883, -15.42029508461213716, 6.325359435864005064 ) ) ;
#15929 = CARTESIAN_POINT ( 'NONE',  ( 12.62599079447150885, -20.19996487918709249, 4.820256282269618886 ) ) ;
#15930 = CARTESIAN_POINT ( 'NONE',  ( -14.49999999999999645, -21.00000000000000355, 4.000000000000000000 ) ) ;
#15931 = EDGE_LOOP ( 'NONE', ( #1794, #4719, #11682, #11786 ) ) ;
#15932 = VERTEX_POINT ( 'NONE', #10890 ) ;
#15933 = CARTESIAN_POINT ( 'NONE',  ( -7.500000000000000888, -9.999999999999992895, 2.500000000000000000 ) ) ;
#15934 = CARTESIAN_POINT ( 'NONE',  ( -24.12918902992234393, 0.000000000000000000, 0.000000000000000000 ) ) ;
#15935 = AXIS2_PLACEMENT_3D ( 'NONE', #15812, #12564, #18964 ) ;
#15936 = DIRECTION ( 'NONE',  ( -1.000000000000000000, -0.000000000000000000, 0.000000000000000000 ) ) ;
#15937 = CARTESIAN_POINT ( 'NONE',  ( 2.583953725994688533, -9.847075946378776479, 2.560676788604062004 ) ) ;
#15938 = LINE ( 'NONE', #16163, #4984 ) ;
#15939 = CARTESIAN_POINT ( 'NONE',  ( 1.897597015127918230, -9.924601616748528699, 1.637971946730535588 ) ) ;
#15940 = DIRECTION ( 'NONE',  ( 1.000000000000000000, 0.000000000000000000, 0.000000000000000000 ) ) ;
#15941 = DIRECTION ( 'NONE',  ( -0.000000000000000000, -0.000000000000000000, -1.000000000000000000 ) ) ;
#15942 = LINE ( 'NONE', #11242, #9016 ) ;
#15943 = CARTESIAN_POINT ( 'NONE',  ( 27.94203811574921659, 9.999999999999998224, 1.000000000000000000 ) ) ;
#15944 = CARTESIAN_POINT ( 'NONE',  ( -3.500698171653725765, 10.00000000000000000, 0.000000000000000000 ) ) ;
#15945 = CARTESIAN_POINT ( 'NONE',  ( -2.534747216115884161, -9.671180236796224960, 2.515503256513427210 ) ) ;
#15946 = CARTESIAN_POINT ( 'NONE',  ( 12.05905858231679595, -21.25705176302045274, 4.171265325393551215 ) ) ;
#15947 = CARTESIAN_POINT ( 'NONE',  ( -13.08739618700683849, 3.851007443844064237, 5.254256565007597857 ) ) ;
#15948 = CARTESIAN_POINT ( 'NONE',  ( -6.902808582316795949, -22.46490103525074034, 2.520995438708341307 ) ) ;
#15949 = EDGE_CURVE ( 'NONE', #7068, #19990, #2617, .T. ) ;
#15950 = CARTESIAN_POINT ( 'NONE',  ( -5.315941417683176518, -20.26807450282663225, 5.303608408759377113 ) ) ;
#15951 = ORIENTED_EDGE ( 'NONE', *, *, #12473, .T. ) ;
#15952 = CARTESIAN_POINT ( 'NONE',  ( 13.08739618700683849, 3.851007443844064237, 5.254256565007597857 ) ) ;
#15953 = DIRECTION ( 'NONE',  ( 0.000000000000000000, 0.000000000000000000, -1.000000000000000000 ) ) ;
#15954 = EDGE_LOOP ( 'NONE', ( #7790, #5486, #13494, #7297, #4953, #9534, #7891, #5603 ) ) ;
#15955 = ORIENTED_EDGE ( 'NONE', *, *, #2861, .T. ) ;
#15956 = CARTESIAN_POINT ( 'NONE',  ( 21.67243175760212637, 9.000000000000001776, 0.000000000000000000 ) ) ;
#15957 = ORIENTED_EDGE ( 'NONE', *, *, #17569, .F. ) ;
#15958 = DIRECTION ( 'NONE',  ( 0.000000000000000000, 1.000000000000000000, 0.000000000000000000 ) ) ;
#15959 = AXIS2_PLACEMENT_3D ( 'NONE', #18082, #2076, #3844 ) ;
#15960 = VECTOR ( 'NONE', #5715, 1000.000000000000000 ) ;
#15961 = PRODUCT_DEFINITION ( 'UNKNOWN', '', #7040, #4614 ) ;
#15962 = VERTEX_POINT ( 'NONE', #4506 ) ;
#15963 = CARTESIAN_POINT ( 'NONE',  ( 12.25344141768317741, -21.94931252712233061, 1.749999999999998446 ) ) ;
#15964 = DIRECTION ( 'NONE',  ( -0.000000000000000000, -0.000000000000000000, -1.000000000000000000 ) ) ;
#15965 = CARTESIAN_POINT ( 'NONE',  ( -2.645259258103298983, -10.28229522185712241, 2.672449792925449596 ) ) ;
#15966 = CARTESIAN_POINT ( 'NONE',  ( -30.00000000000000000, 0.000000000000000000, 1.000000000000000000 ) ) ;
#15967 = CARTESIAN_POINT ( 'NONE',  ( -12.15280858231679595, -21.22443879296942626, 5.229004561291660025 ) ) ;
#15968 = VECTOR ( 'NONE', #18822, 1000.000000000000000 ) ;
#15969 = LINE ( 'NONE', #9806, #13970 ) ;
#15970 = CARTESIAN_POINT ( 'NONE',  ( 6.534691417683177406, -19.47900456129164581, 2.515153566944927199 ) ) ;
#15971 = VECTOR ( 'NONE', #11370, 1000.000000000000000 ) ;
#15972 = CARTESIAN_POINT ( 'NONE',  ( -13.12529397354238192, 5.014845663890295846, 4.333333333333382775 ) ) ;
#15973 = CARTESIAN_POINT ( 'NONE',  ( -6.722191417683177406, -20.27099543870833998, 4.275561207030583510 ) ) ;
#15974 = VERTEX_POINT ( 'NONE', #2933 ) ;
#15975 = CARTESIAN_POINT ( 'NONE',  ( 4.934058582316793284, -23.20159541128345992, 4.773278322869455970 ) ) ;
#15976 = FACE_OUTER_BOUND ( 'NONE', #18526, .T. ) ;
#15977 = CARTESIAN_POINT ( 'NONE',  ( -12.81251082758882376, -11.53070320674076576, 6.423537912489145185 ) ) ;
#15978 = ORIENTED_EDGE ( 'NONE', *, *, #16904, .F. ) ;
#15979 = EDGE_CURVE ( 'NONE', #14618, #2750, #14030, .T. ) ;
#15980 = CARTESIAN_POINT ( 'NONE',  ( 7.934058582316792396, -23.20159541128345992, 4.773278322869455970 ) ) ;
#15981 = CARTESIAN_POINT ( 'NONE',  ( 6.183390479346035917, 4.999999999999999112, 1.000000000000000000 ) ) ;
#15982 = VERTEX_POINT ( 'NONE', #1065 ) ;
#15983 = AXIS2_PLACEMENT_3D ( 'NONE', #16795, #801, #11669 ) ;
#15984 = LINE ( 'NONE', #15783, #19966 ) ;
#15985 = APPLICATION_PROTOCOL_DEFINITION ( 'draft international standard', 'automotive_design', 1998, #15087 ) ;
#15986 = VERTEX_POINT ( 'NONE', #18738 ) ;
#15987 = VECTOR ( 'NONE', #12599, 1000.000000000000000 ) ;
#15988 = DIRECTION ( 'NONE',  ( 1.000000000000000000, 0.000000000000000000, 0.000000000000000000 ) ) ;
#15989 = ADVANCED_FACE ( 'NONE', ( #14211 ), #12545, .T. ) ;
#15990 = EDGE_CURVE ( 'NONE', #14162, #9049, #1371, .T. ) ;
#15991 = VECTOR ( 'NONE', #12113, 1000.000000000000000 ) ;
#15992 = ORIENTED_EDGE ( 'NONE', *, *, #14365, .T. ) ;
#15993 = CARTESIAN_POINT ( 'NONE',  ( -4.687312169500632564, -21.51559725698341197, 5.182386163300427562 ) ) ;
#15994 = LINE ( 'NONE', #1468, #16279 ) ;
#15995 = DIRECTION ( 'NONE',  ( 0.000000000000000000, 1.000000000000000000, 0.000000000000000000 ) ) ;
#15996 = CARTESIAN_POINT ( 'NONE',  ( 1.126276606324276619, -9.864917468222230923, 1.622643865078341907 ) ) ;
#15997 = PLANE ( 'NONE',  #12725 ) ;
#15998 = CARTESIAN_POINT ( 'NONE',  ( -13.37499999999998401, -20.24999999999998934, 2.439580858552613751 ) ) ;
#15999 = AXIS2_PLACEMENT_3D ( 'NONE', #18142, #665, #7054 ) ;
#16000 = VECTOR ( 'NONE', #1446, 1000.000000000000000 ) ;
#16001 = CARTESIAN_POINT ( 'NONE',  ( 6.996558582316793284, -22.05068747287764452, 1.749999999999998446 ) ) ;
#16002 = CARTESIAN_POINT ( 'NONE',  ( -12.65816212372154403, -19.32531275206247301, 6.255900543948403225 ) ) ;
#16003 = AXIS2_PLACEMENT_3D ( 'NONE', #2923, #9301, #17350 ) ;
#16004 = LINE ( 'NONE', #12761, #13373 ) ;
#16005 = CARTESIAN_POINT ( 'NONE',  ( -6.902808582316795949, -23.08622137881038938, 1.020995438708339309 ) ) ;
#16006 = CARTESIAN_POINT ( 'NONE',  ( 6.809058582316794173, -23.27327832286945153, 2.298404588716537411 ) ) ;
#16007 = VECTOR ( 'NONE', #4456, 1000.000000000000000 ) ;
#16008 = ADVANCED_FACE ( 'NONE', ( #14117 ), #9113, .T. ) ;
#16009 = CARTESIAN_POINT ( 'NONE',  ( 5.597191417683177406, -22.46490103525075810, 4.479004561291653808 ) ) ;
#16010 = CARTESIAN_POINT ( 'NONE',  ( -7.190941417683176518, -23.27327832286946219, 4.701595411283453707 ) ) ;
#16011 = ORIENTED_EDGE ( 'NONE', *, *, #9408, .T. ) ;
#16012 = ORIENTED_EDGE ( 'NONE', *, *, #5913, .T. ) ;
#16013 = CARTESIAN_POINT ( 'NONE',  ( 13.84137125862932649, 4.051748560779529384, 5.236069268230914453 ) ) ;
#16014 = CARTESIAN_POINT ( 'NONE',  ( 2.687849085826861995, 10.00000000000000000, 0.000000000000000000 ) ) ;
#16015 = DIRECTION ( 'NONE',  ( 0.000000000000000000, 0.000000000000000000, 1.000000000000000000 ) ) ;
#16016 = ORIENTED_EDGE ( 'NONE', *, *, #20383, .F. ) ;
#16017 = ORIENTED_EDGE ( 'NONE', *, *, #10426, .F. ) ;
#16018 = CARTESIAN_POINT ( 'NONE',  ( 5.000000000000000000, -7.500000000000000000, 3.160254037844365094 ) ) ;
#16019 = EDGE_CURVE ( 'NONE', #9844, #12110, #13806, .T. ) ;
#16020 = VECTOR ( 'NONE', #10842, 1000.000000000000000 ) ;
#16021 = ADVANCED_FACE ( 'NONE', ( #20420 ), #12644, .T. ) ;
#16022 = FACE_BOUND ( 'NONE', #16155, .T. ) ;
#16023 = DIRECTION ( 'NONE',  ( -3.469446951953611033E-15, -1.000000000000000000, 0.000000000000000000 ) ) ;
#16024 = VECTOR ( 'NONE', #6214, 1000.000000000000000 ) ;
#16025 = CARTESIAN_POINT ( 'NONE',  ( -3.292205091070697698, -9.639507599131205140, 2.699984073191874057 ) ) ;
#16026 = DIRECTION ( 'NONE',  ( -0.000000000000000000, 0.000000000000000000, -1.000000000000000000 ) ) ;
#16027 = VECTOR ( 'NONE', #11905, 1000.000000000000000 ) ;
#16028 = DIRECTION ( 'NONE',  ( 1.000000000000000000, 0.000000000000000000, 0.000000000000000000 ) ) ;
#16029 = CARTESIAN_POINT ( 'NONE',  ( -12.66849571425264287, -18.05346643024382303, 5.533233176248494978 ) ) ;
#16030 = CARTESIAN_POINT ( 'NONE',  ( -24.79469207716615031, 4.999999999999999112, 1.000000000000000000 ) ) ;
#16031 = CARTESIAN_POINT ( 'NONE',  ( -14.99999999999998579, -18.49999999999999645, 4.000000000000000000 ) ) ;
#16032 = CARTESIAN_POINT ( 'NONE',  ( 12.62499999998404121, -20.24999999996810729, 2.793053905886972998 ) ) ;
#16033 = CARTESIAN_POINT ( 'NONE',  ( -1.513434189748285918, -9.864917468222230923, 1.622643865078341907 ) ) ;
#16034 = ORIENTED_EDGE ( 'NONE', *, *, #13948, .T. ) ;
#16035 = AXIS2_PLACEMENT_3D ( 'NONE', #7998, #20360, #9468 ) ;
#16036 = CARTESIAN_POINT ( 'NONE',  ( -13.87470602645761986, 4.985154336109792972, 3.000000000000000000 ) ) ;
#16037 = DIRECTION ( 'NONE',  ( -0.1736481776669293042, 0.9848077530122082424, 0.000000000000000000 ) ) ;
#16038 = EDGE_CURVE ( 'NONE', #10986, #2075, #18632, .T. ) ;
#16039 = CARTESIAN_POINT ( 'NONE',  ( 4.565941417683176518, -23.73192549717336064, 1.696391591240623331 ) ) ;
#16040 = CARTESIAN_POINT ( 'NONE',  ( -10.74655858231679595, -21.94931252712234127, 4.499999999999999112 ) ) ;
#16041 = VECTOR ( 'NONE', #10653, 1000.000000000000000 ) ;
#16042 = EDGE_LOOP ( 'NONE', ( #2175, #793, #13632, #4895 ) ) ;
#16043 = ADVANCED_FACE ( 'NONE', ( #1266 ), #17880, .F. ) ;
#16044 = CARTESIAN_POINT ( 'NONE',  ( 12.62527129584495000, -20.98629955982801576, 4.726243163759704657 ) ) ;
#16045 = CARTESIAN_POINT ( 'NONE',  ( 12.91308523408712183, -5.701695678577235249, 5.798858176249892082 ) ) ;
#16046 = CARTESIAN_POINT ( 'NONE',  ( 1.937849085826861328, 11.64110105645932691, 0.000000000000000000 ) ) ;
#16047 = ORIENTED_EDGE ( 'NONE', *, *, #20231, .T. ) ;
#16048 = VECTOR ( 'NONE', #14551, 1000.000000000000000 ) ;
#16049 = ORIENTED_EDGE ( 'NONE', *, *, #18891, .T. ) ;
#16050 = LINE ( 'NONE', #19302, #11768 ) ;
#16051 = LINE ( 'NONE', #13114, #16914 ) ;
#16052 = DIRECTION ( 'NONE',  ( -1.000000000000000000, 0.000000000000000000, 0.000000000000000000 ) ) ;
#16053 = EDGE_CURVE ( 'NONE', #19576, #2967, #12754, .T. ) ;
#16054 = AXIS2_PLACEMENT_3D ( 'NONE', #9717, #16101, #11387 ) ;
#16055 = DIRECTION ( 'NONE',  ( 1.734723475976809067E-16, -1.000000000000000000, 0.000000000000000000 ) ) ;
#16056 = CARTESIAN_POINT ( 'NONE',  ( 1.548630333695928618, -9.864917468222230923, 1.622643865078341907 ) ) ;
#16057 = PLANE ( 'NONE',  #4193 ) ;
#16058 = CARTESIAN_POINT ( 'NONE',  ( 11.00000000000000000, -18.49999999999999645, 6.500000000000000888 ) ) ;
#16059 = CIRCLE ( 'NONE', #15382, 0.5000000000000000000 ) ;
#16060 = VECTOR ( 'NONE', #4126, 1000.000000000000000 ) ;
#16061 = DIRECTION ( 'NONE',  ( -0.000000000000000000, -0.000000000000000000, -1.000000000000000000 ) ) ;
#16062 = CARTESIAN_POINT ( 'NONE',  ( -20.00000000000000000, 3.499999999999999556, 1.500000000000000000 ) ) ;
#16063 = CARTESIAN_POINT ( 'NONE',  ( -11.40280858231679417, -22.77556120703056308, 1.770995438708339975 ) ) ;
#16064 = CARTESIAN_POINT ( 'NONE',  ( -1.407845757905374695, -9.114917468222230923, 2.372643865078341019 ) ) ;
#16065 = CARTESIAN_POINT ( 'NONE',  ( 11.87155858231679595, -20.99999999999999645, 3.449312527122348371 ) ) ;
#16066 = CARTESIAN_POINT ( 'NONE',  ( -13.01365964058540037, 0.1273118495903458325, 5.174178440007729307 ) ) ;
#16067 = CARTESIAN_POINT ( 'NONE',  ( -6.434058582316796837, -22.67126532539354855, 4.242948236979545484 ) ) ;
#16068 = EDGE_CURVE ( 'NONE', #11811, #13228, #11096, .T. ) ;
#16069 = CARTESIAN_POINT ( 'NONE',  ( -5.034691417683177406, -19.47900456129164581, 2.515153566944927199 ) ) ;
#16070 = VERTEX_POINT ( 'NONE', #9926 ) ;
#16071 = EDGE_CURVE ( 'NONE', #17458, #11469, #17467, .T. ) ;
#16072 = CARTESIAN_POINT ( 'NONE',  ( 13.84256985046264710, 4.112277448363203192, 5.213861325540929847 ) ) ;
#16073 = DIRECTION ( 'NONE',  ( -0.000000000000000000, -0.000000000000000000, -1.000000000000000000 ) ) ;
#16074 = ORIENTED_EDGE ( 'NONE', *, *, #1538, .F. ) ;
#16075 = ORIENTED_EDGE ( 'NONE', *, *, #7869, .T. ) ;
#16076 = CARTESIAN_POINT ( 'NONE',  ( 5.000000000000000000, -7.500000000000000000, 3.160254037844365094 ) ) ;
#16077 = VERTEX_POINT ( 'NONE', #4705 ) ;
#16078 = PLANE ( 'NONE',  #19809 ) ;
#16079 = VECTOR ( 'NONE', #4839, 1000.000000000000000 ) ;
#16080 = VECTOR ( 'NONE', #3883, 1000.000000000000000 ) ;
#16081 = ORIENTED_EDGE ( 'NONE', *, *, #14481, .F. ) ;
#16082 = CARTESIAN_POINT ( 'NONE',  ( 8.878441417683177406, -23.74999999999999645, 3.449312527122335492 ) ) ;
#16083 = EDGE_CURVE ( 'NONE', #49, #18833, #10519, .T. ) ;
#16084 = DIRECTION ( 'NONE',  ( -0.000000000000000000, 0.000000000000000000, -1.000000000000000000 ) ) ;
#16085 = CARTESIAN_POINT ( 'NONE',  ( -0.5631383031621635116, -9.114917468222230923, 2.372643865078341019 ) ) ;
#16086 = CARTESIAN_POINT ( 'NONE',  ( 3.047379876266447685, -13.13734219723468755, 3.405682891496055742 ) ) ;
#16087 = DIRECTION ( 'NONE',  ( -0.000000000000000000, -0.000000000000000000, -1.000000000000000000 ) ) ;
#16088 = CARTESIAN_POINT ( 'NONE',  ( 2.687849085826861995, 0.000000000000000000, 1.000000000000000000 ) ) ;
#16089 = CARTESIAN_POINT ( 'NONE',  ( 7.753441417683176518, -21.94931252712233061, 1.749999999999998446 ) ) ;
#16090 = CARTESIAN_POINT ( 'NONE',  ( 23.31633994409548549, 0.000000000000000000, 0.000000000000000000 ) ) ;
#16091 = CARTESIAN_POINT ( 'NONE',  ( -10.94094141768317741, -21.25705176302044208, 2.828734674606458555 ) ) ;
#16092 = AXIS2_PLACEMENT_3D ( 'NONE', #3154, #9525, #15897 ) ;
#16093 = VERTEX_POINT ( 'NONE', #17671 ) ;
#16094 = CARTESIAN_POINT ( 'NONE',  ( 7.090308582316795061, -21.01515356694490322, 0.9790045612916562501 ) ) ;
#16095 = CARTESIAN_POINT ( 'NONE',  ( 13.10192273101908000, 3.834597916462216816, 6.003936301248457674 ) ) ;
#16096 = CARTESIAN_POINT ( 'NONE',  ( -12.65457057572495181, -19.50668592589112293, 6.238308001337955488 ) ) ;
#16097 = ORIENTED_EDGE ( 'NONE', *, *, #14288, .F. ) ;
#16098 = CARTESIAN_POINT ( 'NONE',  ( 8.965308582316794173, -20.22900456129164937, 4.174186261275266929 ) ) ;
#16099 = DIRECTION ( 'NONE',  ( 1.000000000000000000, 1.013672804646636068E-16, 0.000000000000000000 ) ) ;
#16100 = ORIENTED_EDGE ( 'NONE', *, *, #3482, .F. ) ;
#16101 = DIRECTION ( 'NONE',  ( 0.000000000000000000, 0.000000000000000000, 1.000000000000000000 ) ) ;
#16102 = VERTEX_POINT ( 'NONE', #11191 ) ;
#16103 = LINE ( 'NONE', #7747, #16472 ) ;
#16104 = EDGE_LOOP ( 'NONE', ( #14701, #17655, #10832, #18390, #15782, #3362 ) ) ;
#16105 = CARTESIAN_POINT ( 'NONE',  ( -11.77780858231679595, -19.52099543870833642, 2.413778621189609286 ) ) ;
#16106 = CIRCLE ( 'NONE', #13767, 1.499999999999996225 ) ;
#16107 = LINE ( 'NONE', #1672, #14256 ) ;
#16108 = DIRECTION ( 'NONE',  ( 0.000000000000000000, -0.000000000000000000, 1.000000000000000000 ) ) ;
#16109 = CARTESIAN_POINT ( 'NONE',  ( 2.097836924194969033, -11.64739567274323129, 2.830419876579102212 ) ) ;
#16110 = ADVANCED_FACE ( 'NONE', ( #1567 ), #1878, .F. ) ;
#16111 = CARTESIAN_POINT ( 'NONE',  ( 13.15498530132288479, 5.764257716805535559, 4.166666666666765551 ) ) ;
#16112 = DIRECTION ( 'NONE',  ( 1.000000000000000000, -0.000000000000000000, 0.000000000000000000 ) ) ;
#16113 = CARTESIAN_POINT ( 'NONE',  ( -13.83890698502169059, 3.927302743594121903, 5.241364546715693074 ) ) ;
#16114 = CARTESIAN_POINT ( 'NONE',  ( 10.18405858231679595, -20.26807450282662160, 1.696391591240633101 ) ) ;
#16115 = VECTOR ( 'NONE', #19483, 1000.000000000000000 ) ;
#16116 = CARTESIAN_POINT ( 'NONE',  ( -13.12175473207386922, 4.086113969730903683, 6.756475741440692850 ) ) ;
#16117 = DIRECTION ( 'NONE',  ( 0.000000000000000000, -1.000000000000000000, 0.000000000000000000 ) ) ;
#16118 = CARTESIAN_POINT ( 'NONE',  ( 5.027808582316793284, -23.72900456129165647, 4.275561207030568411 ) ) ;
#16119 = VECTOR ( 'NONE', #10180, 1000.000000000000000 ) ;
#16120 = CARTESIAN_POINT ( 'NONE',  ( 7.378441417683177406, -22.99999999999999645, 3.449312527122335048 ) ) ;
#16121 = CARTESIAN_POINT ( 'NONE',  ( -7.472191417683176518, -23.72900456129164937, 2.724438792969417378 ) ) ;
#16122 = ORIENTED_EDGE ( 'NONE', *, *, #19410, .F. ) ;
#16123 = ORIENTED_EDGE ( 'NONE', *, *, #6668, .F. ) ;
#16124 = CARTESIAN_POINT ( 'NONE',  ( 13.84501469867711698, 4.235742283194553259, 4.583333333333295734 ) ) ;
#16125 = CARTESIAN_POINT ( 'NONE',  ( -24.87918902992234393, 0.000000000000000000, 0.000000000000000000 ) ) ;
#16126 = LINE ( 'NONE', #5032, #6024 ) ;
#16127 = ORIENTED_EDGE ( 'NONE', *, *, #11154, .F. ) ;
#16128 = ORIENTED_EDGE ( 'NONE', *, *, #12166, .F. ) ;
#16129 = CARTESIAN_POINT ( 'NONE',  ( 20.00000000000000000, 3.000000000000004441, 1.500000000000000000 ) ) ;
#16130 = LINE ( 'NONE', #1899, #4023 ) ;
#16131 = CARTESIAN_POINT ( 'NONE',  ( -13.12529397354238192, 5.014845663890295846, 4.583333333333296622 ) ) ;
#16132 = B_SPLINE_CURVE_WITH_KNOTS ( 'NONE', 3,
 ( #4932, #16330, #5554, #16433, #16627, #9948, #10366, #10260, #19490, #16531, #13089, #2414, #6914, #638, #3880, #2304, #18003, #6719, #14761, #8696, #2207, #5240, #2107, #19898, #11519, #15067, #11826, #19584, #18216, #8492, #16742, #13499, #11926, #18319, #6819, #3983, #749, #3782, #11617, #7135, #3675, #10061, #8805, #334, #5455, #14861, #5143, #13188, #17902, #3569, #536, #2004, #8391, #13394, #439, #13284, #19683, #5347, #7027, #11724, #18119, #10160, #8589, #14958, #19798, #2511, #4192, #15379, #20209, #4294, #2932, #18427, #18530, #4091, #10788, #9112, #1163, #15173, #18631, #7335, #8904, #16844, #7543, #1265 ),
 .UNSPECIFIED., .F., .F.,
 ( 4, 2, 2, 2, 2, 2, 2, 2, 2, 2, 2, 2, 2, 2, 2, 2, 2, 2, 2, 2, 2, 2, 2, 2, 2, 2, 2, 2, 2, 2, 2, 2, 2, 2, 2, 2, 2, 2, 2, 2, 2, 4 ),
 ( 0.03313147696908364664, 0.03481082764294501225, 0.05122453910963482154, 0.05943139484297972619, 0.06353482270965217504, 0.06763825057632462390, 0.07081696859385247511, 0.07399568661138032633, 0.08035312264643604263, 0.09306799471654744749, 0.1057828667866588523, 0.1121403028217145825, 0.1153190208392423921, 0.1184977388567702294, 0.1214804596100246548, 0.1244631803632790801, 0.1304286218697878474, 0.1423595048828054654, 0.1662212709088406182, 0.2139448029609110069, 0.3093918670650517289, 0.5002859952733333948, 0.6911801234816148387, 0.7866271875857556717, 0.8343507196378259216, 0.8582124856638611021, 0.8701433686768788034, 0.8761088101833875985, 0.8790915309366421626, 0.8820742516898965047, 0.8853411830926054549, 0.8886081144953145161, 0.8951419773007325276, 0.9082097029115688835, 0.9212774285224050175, 0.9278112913278232510, 0.9310782227305322012, 0.9343451541332412624, 0.9384485819999136558, 0.9425520098665861601, 0.9507588655999309468, 0.9671725770666207422 ),
 .UNSPECIFIED. ) ;
#16133 = CARTESIAN_POINT ( 'NONE',  ( -1.906542528716098417, -8.376716462152538512, 1.625674082428238298 ) ) ;
#16134 = CARTESIAN_POINT ( 'NONE',  ( 0.000000000000000000, 10.00000000000000000, 1.000000000000000000 ) ) ;
#16135 = VECTOR ( 'NONE', #18313, 1000.000000000000000 ) ;
#16136 = EDGE_CURVE ( 'NONE', #9411, #1583, #12955, .T. ) ;
#16137 = CARTESIAN_POINT ( 'NONE',  ( 0.000000000000000000, 4.999999999999999112, 0.000000000000000000 ) ) ;
#16138 = CARTESIAN_POINT ( 'NONE',  ( -12.63943061533661982, -19.52125392549825733, 5.470334935344855154 ) ) ;
#16139 = CARTESIAN_POINT ( 'NONE',  ( 10.74655858231679417, -21.94931252712234482, 5.250000000000000888 ) ) ;
#16140 = PLANE ( 'NONE',  #2729 ) ;
#16141 = CARTESIAN_POINT ( 'NONE',  ( 12.62499999999998579, -20.24999999999999289, 3.666666666666653640 ) ) ;
#16142 = CARTESIAN_POINT ( 'NONE',  ( -2.067263844777544435, -10.27417889452513933, 1.727750375171331676 ) ) ;
#16143 = EDGE_CURVE ( 'NONE', #7302, #11608, #19358, .T. ) ;
#16144 = ORIENTED_EDGE ( 'NONE', *, *, #3557, .T. ) ;
#16145 = EDGE_CURVE ( 'NONE', #551, #14903, #8368, .T. ) ;
#16146 = CARTESIAN_POINT ( 'NONE',  ( -13.37500000000002132, -21.00000000000274269, 4.083333333315724012 ) ) ;
#16147 = LINE ( 'NONE', #237, #11723 ) ;
#16148 = CARTESIAN_POINT ( 'NONE',  ( 4.003441417683175629, -22.05068747287766229, 6.000000000000001776 ) ) ;
#16149 = VECTOR ( 'NONE', #2391, 1000.000000000000000 ) ;
#16150 = CARTESIAN_POINT ( 'NONE',  ( -5.871558582316795949, -20.99999999999999645, 3.449312527122348371 ) ) ;
#16151 = ORIENTED_EDGE ( 'NONE', *, *, #5100, .F. ) ;
#16152 = CARTESIAN_POINT ( 'NONE',  ( 13.90439735423812273, 5.734566389025032684, 4.583333333333295734 ) ) ;
#16153 = CARTESIAN_POINT ( 'NONE',  ( 12.72125031657057015, -15.38935901321805133, 5.590524842915047365 ) ) ;
#16154 = DIRECTION ( 'NONE',  ( 1.000000000000000000, 0.000000000000000000, -0.000000000000000000 ) ) ;
#16155 = EDGE_LOOP ( 'NONE', ( #12363, #10591, #6766, #20592 ) ) ;
#16156 = CIRCLE ( 'NONE', #5115, 1.499999999999998668 ) ;
#16157 = ORIENTED_EDGE ( 'NONE', *, *, #8649, .T. ) ;
#16158 = DIRECTION ( 'NONE',  ( -0.7071067811865474617, 0.000000000000000000, -0.7071067811865474617 ) ) ;
#16159 = DIRECTION ( 'NONE',  ( 0.000000000000000000, -1.000000000000000000, 0.000000000000000000 ) ) ;
#16160 = ORIENTED_EDGE ( 'NONE', *, *, #16689, .T. ) ;
#16161 = EDGE_CURVE ( 'NONE', #16884, #20045, #5014, .T. ) ;
#16162 = VECTOR ( 'NONE', #20464, 1000.000000000000000 ) ;
#16163 = CARTESIAN_POINT ( 'NONE',  ( 0.000000000000000000, 9.000000000000001776, 1.000000000000000000 ) ) ;
#16164 = CARTESIAN_POINT ( 'NONE',  ( 2.155282726790247239, -12.05525952636828357, 2.935167462089139256 ) ) ;
#16165 = CARTESIAN_POINT ( 'NONE',  ( 13.87500000000000178, 5.000000000000047962, 2.000000000000000000 ) ) ;
#16166 = CARTESIAN_POINT ( 'NONE',  ( 10.49999999999999645, -9.999999999999991118, 2.000000000000000000 ) ) ;
#16167 =( REPRESENTATION_RELATIONSHIP ('NONE','NONE', #1880, #537 ) REPRESENTATION_RELATIONSHIP_WITH_TRANSFORMATION ( #15144 )SHAPE_REPRESENTATION_RELATIONSHIP( ) );
#16168 = DIRECTION ( 'NONE',  ( -1.000000000000000000, -0.000000000000000000, -0.000000000000000000 ) ) ;
#16169 = CARTESIAN_POINT ( 'NONE',  ( -15.11404127825609223, 4.999999999999999112, 0.000000000000000000 ) ) ;
#16170 = CARTESIAN_POINT ( 'NONE',  ( -12.52780858231679595, -23.72900456129165647, 4.275561207030568411 ) ) ;
#16171 = CARTESIAN_POINT ( 'NONE',  ( -1.655860418491166941, -9.114909740826840689, 2.372641880528837621 ) ) ;
#16172 = ORIENTED_EDGE ( 'NONE', *, *, #18812, .T. ) ;
#16173 = CARTESIAN_POINT ( 'NONE',  ( -13.09553549038190567, 4.262042264285192950, 5.042530537310905281 ) ) ;
#16174 = CARTESIAN_POINT ( 'NONE',  ( -10.55905858231679595, -20.72672167713054137, 4.701595411283463477 ) ) ;
#16175 = CARTESIAN_POINT ( 'NONE',  ( -4.565941417683176518, -23.20159541128344927, 2.226721677130534705 ) ) ;
#16176 = VERTEX_POINT ( 'NONE', #17566 ) ;
#16177 = CARTESIAN_POINT ( 'NONE',  ( 13.83973345681288158, 3.969039569021246550, 5.242263935944164288 ) ) ;
#16178 = DIRECTION ( 'NONE',  ( -0.000000000000000000, -0.000000000000000000, -1.000000000000000000 ) ) ;
#16179 = VERTEX_POINT ( 'NONE', #3345 ) ;
#16180 = VERTEX_POINT ( 'NONE', #3240 ) ;
#16181 = DIRECTION ( 'NONE',  ( 0.000000000000000000, 1.000000000000000000, 0.000000000000000000 ) ) ;
#16182 = ORIENTED_EDGE ( 'NONE', *, *, #155, .T. ) ;
#16183 = DIRECTION ( 'NONE',  ( 1.000000000000000000, 0.000000000000000000, 0.000000000000000000 ) ) ;
#16184 = ORIENTED_EDGE ( 'NONE', *, *, #15603, .F. ) ;
#16185 = CARTESIAN_POINT ( 'NONE',  ( 9.909691417683179182, -21.32581373872474373, 5.270995438708348857 ) ) ;
#16186 = LINE ( 'NONE', #1853, #1322 ) ;
#16187 = ADVANCED_FACE ( 'NONE', ( #8164 ), #9723, .T. ) ;
#16188 = ADVANCED_FACE ( 'NONE', ( #14530 ), #8060, .T. ) ;
#16189 = CARTESIAN_POINT ( 'NONE',  ( -0.9854920305337622199, -9.864917468222230923, 2.372643865078341019 ) ) ;
#16190 = LINE ( 'NONE', #9699, #20707 ) ;
#16191 = CARTESIAN_POINT ( 'NONE',  ( -9.527808582316794173, -23.72900456129165292, 4.275561207030568411 ) ) ;
#16192 = ADVANCED_FACE ( 'NONE', ( #19256 ), #3448, .T. ) ;
#16193 = FILL_AREA_STYLE_COLOUR ( '', #16968 ) ;
#16194 = CARTESIAN_POINT ( 'NONE',  ( 7.097191417683177406, -22.77556120703057729, 5.229004561291655584 ) ) ;
#16195 = DIRECTION ( 'NONE',  ( -0.000000000000000000, -0.000000000000000000, -1.000000000000000000 ) ) ;
#16196 = CARTESIAN_POINT ( 'NONE',  ( -11.12844141768317741, -20.99999999999999645, 3.550687472877664952 ) ) ;
#16197 = VERTEX_POINT ( 'NONE', #309 ) ;
#16198 = CARTESIAN_POINT ( 'NONE',  ( 10.37155858231679595, -19.49999999999998934, 3.449312527122348371 ) ) ;
#16199 = CARTESIAN_POINT ( 'NONE',  ( 12.65051119073526564, -18.96168486786632457, 5.513701926248478102 ) ) ;
#16200 = CARTESIAN_POINT ( 'NONE',  ( -13.15384296923648400, 5.706569946443514674, 5.461568745250741763 ) ) ;
#16201 = ORIENTED_EDGE ( 'NONE', *, *, #13952, .F. ) ;
#16202 = EDGE_CURVE ( 'NONE', #12110, #7216, #6695, .T. ) ;
#16203 = DIRECTION ( 'NONE',  ( -0.000000000000000000, -0.000000000000000000, -1.000000000000000000 ) ) ;
#16204 = FACE_OUTER_BOUND ( 'NONE', #9563, .T. ) ;
#16205 = ORIENTED_EDGE ( 'NONE', *, *, #17813, .T. ) ;
#16206 = ORIENTED_EDGE ( 'NONE', *, *, #3114, .F. ) ;
#16207 = CARTESIAN_POINT ( 'NONE',  ( 12.63268481240007546, -20.15932789777624023, 3.549899454067339200 ) ) ;
#16208 = ORIENTED_EDGE ( 'NONE', *, *, #13497, .F. ) ;
#16209 = CARTESIAN_POINT ( 'NONE',  ( -11.96530858231679773, -19.47900456129164937, 4.484846433055089676 ) ) ;
#16210 = CARTESIAN_POINT ( 'NONE',  ( 12.72125031657057015, -15.38935901321805133, 5.590524842915047365 ) ) ;
#16211 = DIRECTION ( 'NONE',  ( -0.000000000000000000, 0.000000000000000000, 1.000000000000000000 ) ) ;
#16212 = AXIS2_PLACEMENT_3D ( 'NONE', #15742, #4859, #6329 ) ;
#16213 = CARTESIAN_POINT ( 'NONE',  ( 12.64323021897839006, -19.32937394158751943, 5.504219675487169283 ) ) ;
#16214 = DIRECTION ( 'NONE',  ( -1.000000000000000000, -0.000000000000000000, -0.000000000000000000 ) ) ;
#16215 = CARTESIAN_POINT ( 'NONE',  ( -13.83411111208379474, 3.685111160228107252, 5.236156213382356484 ) ) ;
#16216 = CARTESIAN_POINT ( 'NONE',  ( 8.027808582316795949, -24.47900456129166358, 4.586221378810390270 ) ) ;
#16217 = CARTESIAN_POINT ( 'NONE',  ( -13.04271272860988340, 0.09449279482665236263, 6.673537912489449830 ) ) ;
#16218 = CARTESIAN_POINT ( 'NONE',  ( -10.37844141768317741, -24.50000000000000000, 3.449312527122335048 ) ) ;
#16219 = PLANE ( 'NONE',  #12723 ) ;
#16220 = LINE ( 'NONE', #8269, #19122 ) ;
#16221 = VECTOR ( 'NONE', #8038, 1000.000000000000000 ) ;
#16222 = ADVANCED_FACE ( 'NONE', ( #5120 ), #8365, .T. ) ;
#16223 = CARTESIAN_POINT ( 'NONE',  ( 7.371558582316795949, -20.99999999999999645, 3.449312527122348371 ) ) ;
#16224 = CARTESIAN_POINT ( 'NONE',  ( -6.628441417683176518, -20.24999999999999289, 3.550687472877664952 ) ) ;
#16225 = ORIENTED_EDGE ( 'NONE', *, *, #8902, .F. ) ;
#16226 = EDGE_LOOP ( 'NONE', ( #4389, #13007, #8825, #6832 ) ) ;
#16227 = CARTESIAN_POINT ( 'NONE',  ( 13.84497512400090891, 4.233743762047977199, 5.032110966142367303 ) ) ;
#16228 = DIRECTION ( 'NONE',  ( -1.000000000000000000, 0.000000000000000000, 0.000000000000000000 ) ) ;
#16229 = DIRECTION ( 'NONE',  ( 0.000000000000000000, 0.000000000000000000, 1.000000000000000000 ) ) ;
#16230 = ORIENTED_EDGE ( 'NONE', *, *, #1822, .T. ) ;
#16231 = ORIENTED_EDGE ( 'NONE', *, *, #18634, .F. ) ;
#16232 = DIRECTION ( 'NONE',  ( 0.000000000000000000, 0.000000000000000000, 1.000000000000000000 ) ) ;
#16233 = CARTESIAN_POINT ( 'NONE',  ( 13.49999999999998401, -25.49999999999999645, 4.000000000000000000 ) ) ;
#16234 = CARTESIAN_POINT ( 'NONE',  ( -13.12503131243110843, 5.001581277770153378, 5.166347330538456184 ) ) ;
#16235 = CARTESIAN_POINT ( 'NONE',  ( 32.65117217603048516, 6.460468870412194420, 1.000000000000000000 ) ) ;
#16236 = CARTESIAN_POINT ( 'NONE',  ( -0.000000000000000000, 10.00000000000000000, 0.000000000000000000 ) ) ;
#16237 = CARTESIAN_POINT ( 'NONE',  ( -12.62745083560477966, -20.12623280195927933, 5.001038150054709419 ) ) ;
#16238 = CARTESIAN_POINT ( 'NONE',  ( 6.527808582316794173, -23.72900456129165292, 4.275561207030568411 ) ) ;
#16239 = DIRECTION ( 'NONE',  ( 1.000000000000000000, 0.000000000000000000, -0.000000000000000000 ) ) ;
#16240 = CARTESIAN_POINT ( 'NONE',  ( 12.63819864697926754, -19.58346832754827105, 5.450273968536036406 ) ) ;
#16241 = CARTESIAN_POINT ( 'NONE',  ( -1.126276606324276619, -9.114917468222230923, 2.372643865078341019 ) ) ;
#16242 = ORIENTED_EDGE ( 'NONE', *, *, #1806, .T. ) ;
#16243 = CARTESIAN_POINT ( 'NONE',  ( -13.86470821076586368, 4.480264643675554659, 5.874551681240599343 ) ) ;
#16244 = DIRECTION ( 'NONE',  ( 1.000000000000000000, 0.000000000000000000, 0.000000000000000000 ) ) ;
#16245 = CARTESIAN_POINT ( 'NONE',  ( 10.37844141768317741, -23.74999999999999645, 3.449312527122335492 ) ) ;
#16246 = CARTESIAN_POINT ( 'NONE',  ( -10.55905858231679595, -21.25705176302045274, 4.171265325393551215 ) ) ;
#16247 = VERTEX_POINT ( 'NONE', #7311 ) ;
#16248 = CARTESIAN_POINT ( 'NONE',  ( 13.90258797164900884, 5.643192568275169130, 5.568788873356017355 ) ) ;
#16249 = CARTESIAN_POINT ( 'NONE',  ( 13.10756170493883310, 4.119366099410778581, 6.001761809183453700 ) ) ;
#16250 = CARTESIAN_POINT ( 'NONE',  ( -13.33402348762467327, -20.05346030977060678, 3.454433009287248613 ) ) ;
#16251 = ORIENTED_EDGE ( 'NONE', *, *, #18029, .F. ) ;
#16252 = EDGE_CURVE ( 'NONE', #10437, #4996, #10236, .T. ) ;
#16253 = EDGE_LOOP ( 'NONE', ( #11085, #12466, #4341, #11274 ) ) ;
#16254 = FACE_OUTER_BOUND ( 'NONE', #9655, .T. ) ;
#16255 = CARTESIAN_POINT ( 'NONE',  ( -27.49999999999999645, -4.770489558936219510E-14, 1.000000000000000000 ) ) ;
#16256 = ADVANCED_FACE ( 'NONE', ( #13370, #19773, #19564, #5634 ), #15249, .F. ) ;
#16257 = CARTESIAN_POINT ( 'NONE',  ( 0.000000000000000000, 11.64110105645932691, 10.00000000000000000 ) ) ;
#16258 = LINE ( 'NONE', #4011, #5989 ) ;
#16259 = CARTESIAN_POINT ( 'NONE',  ( 1.863950040896528604, -9.995453039732266731, 2.406168007552154098 ) ) ;
#16260 = LINE ( 'NONE', #15097, #9389 ) ;
#16261 = CARTESIAN_POINT ( 'NONE',  ( 0.000000000000000000, 4.999999999999999112, 0.000000000000000000 ) ) ;
#16262 = CARTESIAN_POINT ( 'NONE',  ( 0.000000000000000000, 0.000000000000000000, 9.999999999999998224 ) ) ;
#16263 = DIRECTION ( 'NONE',  ( 0.000000000000000000, 1.000000000000000000, 0.000000000000000000 ) ) ;
#16264 = FACE_OUTER_BOUND ( 'NONE', #8988, .T. ) ;
#16265 = CARTESIAN_POINT ( 'NONE',  ( -3.342893013439646843, -9.383962644129466568, 1.884355023724047173 ) ) ;
#16266 = EDGE_LOOP ( 'NONE', ( #3229, #20555, #5088, #14388 ) ) ;
#16267 = CARTESIAN_POINT ( 'NONE',  ( -12.62499999999998224, -19.49999999999991473, 4.333333333333343695 ) ) ;
#16268 = CARTESIAN_POINT ( 'NONE',  ( -13.09030858231679417, -21.32581373872472597, 1.729004561291657582 ) ) ;
#16269 = CARTESIAN_POINT ( 'NONE',  ( -8.878441417683177406, -23.74999999999999645, 3.449312527122335492 ) ) ;
#16270 = VERTEX_POINT ( 'NONE', #11696 ) ;
#16271 = CARTESIAN_POINT ( 'NONE',  ( 13.84500676459759383, 4.235341612176667603, 5.016097456370799179 ) ) ;
#16272 = CARTESIAN_POINT ( 'NONE',  ( -4.315753587183822404, -21.47141115243053378, 5.558207674221720573 ) ) ;
#16273 = ORIENTED_EDGE ( 'NONE', *, *, #4754, .T. ) ;
#16274 = ORIENTED_EDGE ( 'NONE', *, *, #4276, .F. ) ;
#16275 = DIRECTION ( 'NONE',  ( 1.000000000000000000, -0.000000000000000000, -0.000000000000000000 ) ) ;
#16276 = EDGE_CURVE ( 'NONE', #10193, #3754, #6893, .T. ) ;
#16277 = ORIENTED_EDGE ( 'NONE', *, *, #10784, .F. ) ;
#16278 = DIRECTION ( 'NONE',  ( 0.000000000000000000, -0.000000000000000000, 1.000000000000000000 ) ) ;
#16279 = VECTOR ( 'NONE', #17466, 1000.000000000000000 ) ;
#16280 = ORIENTED_EDGE ( 'NONE', *, *, #20472, .T. ) ;
#16281 = CARTESIAN_POINT ( 'NONE',  ( 6.534691417683176518, -20.22900456129164581, 2.825813738724748170 ) ) ;
#16282 = CARTESIAN_POINT ( 'NONE',  ( -4.250698171653726654, 11.64110105645932691, 10.00000000000000000 ) ) ;
#16283 = CARTESIAN_POINT ( 'NONE',  ( -1.548630333695928618, -9.864917468222230923, 2.372643865078341019 ) ) ;
#16284 = CARTESIAN_POINT ( 'NONE',  ( 2.579281110863027582, -9.822567596814183233, 2.554382554832406615 ) ) ;
#16285 = CARTESIAN_POINT ( 'NONE',  ( -8.777808582316792396, -20.27099543870833642, 2.724438792969431589 ) ) ;
#16286 = EDGE_CURVE ( 'NONE', #17877, #12439, #11596, .T. ) ;
#16287 =( LENGTH_UNIT ( ) NAMED_UNIT ( * ) SI_UNIT ( .MILLI., .METRE. ) );
#16288 = CARTESIAN_POINT ( 'NONE',  ( 10.75344141768317741, -21.94931252712233061, 1.749999999999998446 ) ) ;
#16289 = LINE ( 'NONE', #14719, #12196 ) ;
#16290 = CARTESIAN_POINT ( 'NONE',  ( -12.15969141768317918, -22.36352608949543352, 2.479004561291652031 ) ) ;
#16291 = ORIENTED_EDGE ( 'NONE', *, *, #17030, .T. ) ;
#16292 = CARTESIAN_POINT ( 'NONE',  ( 10.27780858231679595, -19.52099543870833642, 2.413778621189609286 ) ) ;
#16293 = CARTESIAN_POINT ( 'NONE',  ( 13.05696142222617695, 1.564051822406025583, 5.955108176248398166 ) ) ;
#16294 = CARTESIAN_POINT ( 'NONE',  ( -12.63943061533661982, -19.52125392549825733, 5.470334935344855154 ) ) ;
#16295 = ORIENTED_EDGE ( 'NONE', *, *, #18172, .F. ) ;
#16296 = DIRECTION ( 'NONE',  ( -1.000000000000000000, 3.469446951953491127E-15, 0.000000000000000000 ) ) ;
#16297 = EDGE_CURVE ( 'NONE', #13178, #13945, #17980, .T. ) ;
#16298 = CARTESIAN_POINT ( 'NONE',  ( -14.49999999999998579, -18.49999999999999645, 4.000000000000000000 ) ) ;
#16299 = ADVANCED_FACE ( 'NONE', ( #4068 ), #11803, .T. ) ;
#16300 = ORIENTED_EDGE ( 'NONE', *, *, #2362, .F. ) ;
#16301 =( NAMED_UNIT ( * ) PLANE_ANGLE_UNIT ( ) SI_UNIT ( $, .RADIAN. ) );
#16302 = ORIENTED_EDGE ( 'NONE', *, *, #5151, .F. ) ;
#16303 = FACE_OUTER_BOUND ( 'NONE', #16792, .T. ) ;
#16304 = EDGE_LOOP ( 'NONE', ( #10929, #10440, #6757, #2100 ) ) ;
#16305 = FACE_OUTER_BOUND ( 'NONE', #10418, .T. ) ;
#16306 = CARTESIAN_POINT ( 'NONE',  ( 15.36404127825609400, 9.000000000000001776, 1.000000000000000000 ) ) ;
#16307 = DIRECTION ( 'NONE',  ( -0.000000000000000000, 0.000000000000000000, 1.000000000000000000 ) ) ;
#16308 = EDGE_CURVE ( 'NONE', #9894, #11041, #13263, .T. ) ;
#16309 = CARTESIAN_POINT ( 'NONE',  ( 12.62499999999998224, -20.25000000000006395, 4.416666666666681174 ) ) ;
#16310 = CARTESIAN_POINT ( 'NONE',  ( 4.647268150594000780, -21.56957941601164563, 4.994152606344886891 ) ) ;
#16311 = CARTESIAN_POINT ( 'NONE',  ( -13.37499999999998224, -20.25000000000006395, 4.416666666666681174 ) ) ;
#16312 = CARTESIAN_POINT ( 'NONE',  ( 11.96530858231679773, -19.47900456129164937, 4.484846433055089676 ) ) ;
#16313 = CARTESIAN_POINT ( 'NONE',  ( -13.12035191997235906, 4.015271958632619764, 6.757839745787993735 ) ) ;
#16314 = CARTESIAN_POINT ( 'NONE',  ( -6.246558582316795949, -21.94931252712234127, 6.000000000000001776 ) ) ;
#16315 = LINE ( 'NONE', #17988, #13730 ) ;
#16316 = LINE ( 'NONE', #3457, #18114 ) ;
#16317 = CARTESIAN_POINT ( 'NONE',  ( 10.46530858231679595, -20.97900456129165647, 3.863526089495444626 ) ) ;
#16318 = CARTESIAN_POINT ( 'NONE',  ( -4.940941417683177406, -20.72672167713052715, 2.298404588716546293 ) ) ;
#16319 = AXIS2_PLACEMENT_3D ( 'NONE', #16843, #19996, #748 ) ;
#16320 = EDGE_LOOP ( 'NONE', ( #18178, #16201, #16017, #890, #5140, #16709 ) ) ;
#16321 = ADVANCED_FACE ( 'NONE', ( #19974 ), #16511, .T. ) ;
#16322 = VERTEX_POINT ( 'NONE', #15042 ) ;
#16323 = CARTESIAN_POINT ( 'NONE',  ( 13.37499999999998224, -20.24999999999998934, 4.166666666666636765 ) ) ;
#16324 = CIRCLE ( 'NONE', #7653, 1.499999999999998668 ) ;
#16325 = CARTESIAN_POINT ( 'NONE',  ( -5.433390479346035029, 0.000000000000000000, 1.000000000000000000 ) ) ;
#16326 = PRESENTATION_STYLE_ASSIGNMENT (( #9944 ) ) ;
#16327 = VERTEX_POINT ( 'NONE', #826 ) ;
#16328 = CARTESIAN_POINT ( 'NONE',  ( -7.869520639128047002, 4.999999999999999112, 1.000000000000000000 ) ) ;
#16329 = DIRECTION ( 'NONE',  ( 3.469446951953611033E-15, -1.000000000000000000, 0.000000000000000000 ) ) ;
#16330 = CARTESIAN_POINT ( 'NONE',  ( 13.37499999999995204, -20.24999999999992184, 3.465895369911768054 ) ) ;
#16331 = CIRCLE ( 'NONE', #18005, 1.499999999999998668 ) ;
#16332 = DIRECTION ( 'NONE',  ( -0.000000000000000000, -0.000000000000000000, -1.000000000000000000 ) ) ;
#16333 = CARTESIAN_POINT ( 'NONE',  ( 2.076833265075072266, -8.407161531158021006, 2.383492984350220389 ) ) ;
#16334 = EDGE_CURVE ( 'NONE', #20148, #6837, #10139, .T. ) ;
#16335 = VECTOR ( 'NONE', #14730, 1000.000000000000000 ) ;
#16336 = CARTESIAN_POINT ( 'NONE',  ( 1.407845757905374695, -9.114917468222230923, 1.622643865078341463 ) ) ;
#16337 = CARTESIAN_POINT ( 'NONE',  ( -13.09892531043291086, 3.683228176858501790, 6.000681092915118420 ) ) ;
#16338 = CARTESIAN_POINT ( 'NONE',  ( 4.746558582316793284, -21.94931252712234482, 5.250000000000000888 ) ) ;
#16339 = CARTESIAN_POINT ( 'NONE',  ( -13.81494360078803396, 10.00000000000000000, 1.000000000000000000 ) ) ;
#16340 = CARTESIAN_POINT ( 'NONE',  ( 13.12529418130016445, 5.014856155665242454, 4.958178834604180629 ) ) ;
#16341 = CARTESIAN_POINT ( 'NONE',  ( -2.645259258103298983, -10.28229522185712241, 2.672449792925449596 ) ) ;
#16342 = FACE_OUTER_BOUND ( 'NONE', #1130, .T. ) ;
#16343 = CARTESIAN_POINT ( 'NONE',  ( 11.31594141768317741, -20.79840458871654363, 4.773278322869464851 ) ) ;
#16344 = CARTESIAN_POINT ( 'NONE',  ( -9.434058582316795949, -22.67126532539354855, 4.242948236979545484 ) ) ;
#16345 = EDGE_LOOP ( 'NONE', ( #19432, #5258, #13979, #18931, #2985, #14472 ) ) ;
#16346 = CARTESIAN_POINT ( 'NONE',  ( 13.82120031190154208, 1.533115751011936867, 6.689942769197355865 ) ) ;
#16347 = CARTESIAN_POINT ( 'NONE',  ( 12.83635126708105823, -9.576761012430582198, 5.715524842913705328 ) ) ;
#16348 = VECTOR ( 'NONE', #11644, 1000.000000000000000 ) ;
#16349 = CARTESIAN_POINT ( 'NONE',  ( -13.37327929115833491, -20.24999999560066399, 3.449077790995343840 ) ) ;
#16350 = VERTEX_POINT ( 'NONE', #5217 ) ;
#16351 = VECTOR ( 'NONE', #14570, 1000.000000000000000 ) ;
#16352 = EDGE_LOOP ( 'NONE', ( #5338, #11187, #9222, #9818 ) ) ;
#16353 = CARTESIAN_POINT ( 'NONE',  ( 26.69203811574920238, 10.00000000000000000, 1.000000000000000000 ) ) ;
#16354 = CARTESIAN_POINT ( 'NONE',  ( -0.000000000000000000, 11.64110105645932691, 0.000000000000000000 ) ) ;
#16355 = CARTESIAN_POINT ( 'NONE',  ( -7.500000000000000000, -23.83493649053891517, 4.999999999999999112 ) ) ;
#16356 = CARTESIAN_POINT ( 'NONE',  ( -14.99999999999999645, -30.00000000000000711, 0.000000000000000000 ) ) ;
#16357 = CARTESIAN_POINT ( 'NONE',  ( 1.513434189748285918, -9.864917468222230923, 1.622643865078341907 ) ) ;
#16358 = FACE_OUTER_BOUND ( 'NONE', #18159, .T. ) ;
#16359 = AXIS2_PLACEMENT_3D ( 'NONE', #226, #1801, #1590 ) ;
#16360 = PLANE ( 'NONE',  #12055 ) ;
#16361 = EDGE_CURVE ( 'NONE', #3716, #11889, #17138, .T. ) ;
#16362 = CARTESIAN_POINT ( 'NONE',  ( 13.24898903296832486, -20.53044634143503444, 3.466065607697936368 ) ) ;
#16363 = CARTESIAN_POINT ( 'NONE',  ( -15.87779268661489773, 0.000000000000000000, 1.000000000000000000 ) ) ;
#16364 = CARTESIAN_POINT ( 'NONE',  ( -7.840308582316794173, -22.67418626127525982, 5.270995438708342640 ) ) ;
#16365 = CARTESIAN_POINT ( 'NONE',  ( -1.548630333695928618, -8.364917468222230923, 2.372643865078341019 ) ) ;
#16366 = EDGE_LOOP ( 'NONE', ( #20047, #6884, #1061, #12278 ) ) ;
#16367 = CARTESIAN_POINT ( 'NONE',  ( -12.70672377255832686, -15.37294948583620346, 4.840845106674187548 ) ) ;
#16368 = CARTESIAN_POINT ( 'NONE',  ( -7.184058582316794173, -20.79840458871652942, 2.226721677130544030 ) ) ;
#16369 = CIRCLE ( 'NONE', #6360, 10.00000000000000000 ) ;
#16370 = CARTESIAN_POINT ( 'NONE',  ( -7.940941417683176518, -20.72672167713052715, 2.298404588716546293 ) ) ;
#16371 = VERTEX_POINT ( 'NONE', #19660 ) ;
#16372 = CARTESIAN_POINT ( 'NONE',  ( 13.40368151590352497, -18.05158344687463412, 4.768708296715732153 ) ) ;
#16373 = PLANE ( 'NONE',  #14373 ) ;
#16374 = ORIENTED_EDGE ( 'NONE', *, *, #17838, .F. ) ;
#16375 = ORIENTED_EDGE ( 'NONE', *, *, #12700, .T. ) ;
#16376 = LINE ( 'NONE', #13230, #18771 ) ;
#16377 = VERTEX_POINT ( 'NONE', #2488 ) ;
#16378 = CARTESIAN_POINT ( 'NONE',  ( -13.39296152110871851, -19.34294318400601753, 5.489418334493660012 ) ) ;
#16379 = AXIS2_PLACEMENT_3D ( 'NONE', #1142, #4169, #2281 ) ;
#16380 = EDGE_LOOP ( 'NONE', ( #11389, #17047, #13890, #18470 ) ) ;
#16381 = CARTESIAN_POINT ( 'NONE',  ( 6.440941417683176518, -20.72672167713052715, 2.298404588716546293 ) ) ;
#16382 = CARTESIAN_POINT ( 'NONE',  ( -13.49999999999998401, -18.49999999999999645, 4.000000000000000000 ) ) ;
#16383 = VECTOR ( 'NONE', #2995, 1000.000000000000000 ) ;
#16384 = LINE ( 'NONE', #8754, #10316 ) ;
#16385 = LINE ( 'NONE', #19442, #19034 ) ;
#16386 = CARTESIAN_POINT ( 'NONE',  ( -7.184058582316794173, -20.79840458871652942, 2.226721677130544030 ) ) ;
#16387 = EDGE_CURVE ( 'NONE', #12514, #10855, #13571, .T. ) ;
#16388 = PLANE ( 'NONE',  #613 ) ;
#16389 = CARTESIAN_POINT ( 'NONE',  ( 8.034691417683175629, -20.22900456129164581, 2.825813738724747726 ) ) ;
#16390 = CARTESIAN_POINT ( 'NONE',  ( 15.50000000000002132, -26.49999999999999645, 4.000000000000000000 ) ) ;
#16391 = CARTESIAN_POINT ( 'NONE',  ( -12.06594141768317741, -22.67126532539353789, 2.757051763020445634 ) ) ;
#16392 = CARTESIAN_POINT ( 'NONE',  ( -8.027808582316795949, -24.47900456129166358, 4.586221378810390270 ) ) ;
#16393 = EDGE_LOOP ( 'NONE', ( #1840, #7318, #6836, #11137 ) ) ;
#16394 = EDGE_CURVE ( 'NONE', #6239, #13354, #13474, .T. ) ;
#16395 = CARTESIAN_POINT ( 'NONE',  ( 12.62562019941893432, -20.21867992933967173, 4.757612834768309540 ) ) ;
#16396 = CARTESIAN_POINT ( 'NONE',  ( -13.13728495444130751, 4.870390199291127153, 6.548325014280736767 ) ) ;
#16397 = VECTOR ( 'NONE', #17574, 1000.000000000000000 ) ;
#16398 = ORIENTED_EDGE ( 'NONE', *, *, #10224, .F. ) ;
#16399 = ADVANCED_FACE ( 'NONE', ( #5531 ), #923, .T. ) ;
#16400 = VECTOR ( 'NONE', #18775, 1000.000000000000000 ) ;
#16401 = CARTESIAN_POINT ( 'NONE',  ( -20.00000000000000000, 0.000000000000000000, 2.000000000000000000 ) ) ;
#16402 = FACE_OUTER_BOUND ( 'NONE', #11998, .T. ) ;
#16403 = VECTOR ( 'NONE', #12347, 1000.000000000000000 ) ;
#16404 = EDGE_LOOP ( 'NONE', ( #7542, #4135, #11270, #7072 ) ) ;
#16405 = ORIENTED_EDGE ( 'NONE', *, *, #4350, .T. ) ;
#16406 = CARTESIAN_POINT ( 'NONE',  ( 12.75111466187344966, -19.96946164605619245, 3.533920058977110479 ) ) ;
#16407 = ORIENTED_EDGE ( 'NONE', *, *, #16659, .F. ) ;
#16408 = DIRECTION ( 'NONE',  ( -1.000000000000000000, 0.000000000000000000, 0.000000000000000000 ) ) ;
#16409 = CARTESIAN_POINT ( 'NONE',  ( 0.000000000000000000, 0.000000000000000000, 1.000000000000000000 ) ) ;
#16410 = CARTESIAN_POINT ( 'NONE',  ( -13.49999999999998401, -21.99999999999999645, 11.68378559369222280 ) ) ;
#16411 = VECTOR ( 'NONE', #13505, 1000.000000000000000 ) ;
#16412 = EDGE_CURVE ( 'NONE', #13481, #13250, #616, .T. ) ;
#16413 = CARTESIAN_POINT ( 'NONE',  ( 12.74043380832193684, -14.42059267975384529, 5.611358176248560703 ) ) ;
#16414 = CARTESIAN_POINT ( 'NONE',  ( 20.49999999999998224, -21.99999999999999645, 11.00000000000000178 ) ) ;
#16415 = CARTESIAN_POINT ( 'NONE',  ( 11.30905858231679595, -23.80360840875935935, 1.768074502826626260 ) ) ;
#16416 = CARTESIAN_POINT ( 'NONE',  ( -12.62500016093973620, -20.24999187254239175, 4.532396751752561848 ) ) ;
#16417 = CARTESIAN_POINT ( 'NONE',  ( -10.75344141768317741, -21.94931252712233061, 0.9999999999999978906 ) ) ;
#16418 = CARTESIAN_POINT ( 'NONE',  ( 0.000000000000000000, 0.000000000000000000, 0.000000000000000000 ) ) ;
#16419 = DIRECTION ( 'NONE',  ( 1.000000000000000000, 0.000000000000000000, -0.000000000000000000 ) ) ;
#16420 = CARTESIAN_POINT ( 'NONE',  ( 12.05905858231679595, -21.25705176302045274, 4.171265325393551215 ) ) ;
#16421 = CARTESIAN_POINT ( 'NONE',  ( -4.097191417683176518, -22.77556120703057729, 5.229004561291656472 ) ) ;
#16422 = ORIENTED_EDGE ( 'NONE', *, *, #5438, .F. ) ;
#16423 = ORIENTED_EDGE ( 'NONE', *, *, #7078, .T. ) ;
#16424 = CARTESIAN_POINT ( 'NONE',  ( 13.86106797245302147, 4.296432608878145487, 5.947261916831099171 ) ) ;
#16425 = DIRECTION ( 'NONE',  ( -0.000000000000000000, -0.000000000000000000, -1.000000000000000000 ) ) ;
#16426 =( NAMED_UNIT ( * ) PLANE_ANGLE_UNIT ( ) SI_UNIT ( $, .RADIAN. ) );
#16427 = EDGE_LOOP ( 'NONE', ( #19652, #20041, #19345, #14643 ) ) ;
#16428 = EDGE_CURVE ( 'NONE', #13538, #12998, #2282, .T. ) ;
#16429 = VECTOR ( 'NONE', #17240, 1000.000000000000000 ) ;
#16430 = CARTESIAN_POINT ( 'NONE',  ( 0.000000000000000000, 4.999999999999999112, 1.000000000000000000 ) ) ;
#16431 = CARTESIAN_POINT ( 'NONE',  ( -22.85856191738413656, 9.000000000000001776, 1.000000000000000000 ) ) ;
#16432 = CARTESIAN_POINT ( 'NONE',  ( 0.000000000000000000, 9.000000000000001776, 1.000000000000000000 ) ) ;
#16433 = CARTESIAN_POINT ( 'NONE',  ( 13.37499999999998579, -20.24999999999999289, 3.666666666666653640 ) ) ;
#16434 = DIRECTION ( 'NONE',  ( 0.000000000000000000, -0.000000000000000000, 1.000000000000000000 ) ) ;
#16435 = CARTESIAN_POINT ( 'NONE',  ( 3.882031223148668886, -13.81156101447257889, 3.771450735391772557 ) ) ;
#16436 = EDGE_CURVE ( 'NONE', #14361, #4739, #3956, .T. ) ;
#16437 = EDGE_CURVE ( 'NONE', #5735, #18810, #15664, .T. ) ;
#16438 = CARTESIAN_POINT ( 'NONE',  ( 10.18924542913430820, 0.000000000000000000, 0.000000000000000000 ) ) ;
#16439 = CARTESIAN_POINT ( 'NONE',  ( -12.62599452815238443, -19.44977632830967806, 4.656396506304353977 ) ) ;
#16440 = CARTESIAN_POINT ( 'NONE',  ( 8.684058582316794173, -20.79840458871652942, 2.226721677130544030 ) ) ;
#16441 = CARTESIAN_POINT ( 'NONE',  ( -0.000000000000000000, 10.00000000000000000, 0.000000000000000000 ) ) ;
#16442 = CARTESIAN_POINT ( 'NONE',  ( 12.64931222250080545, -19.02223276370786209, 5.512399842915133519 ) ) ;
#16443 = VECTOR ( 'NONE', #3726, 1000.000000000000000 ) ;
#16444 = B_SPLINE_CURVE_WITH_KNOTS ( 'NONE', 3,
 ( #16655, #13313, #19714, #16555, #8615, #11851 ),
 .UNSPECIFIED., .F., .F.,
 ( 4, 2, 4 ),
 ( 0.000000000000000000, 0.2500000000000000000, 0.5000000000000000000 ),
 .UNSPECIFIED. ) ;
#16445 = CARTESIAN_POINT ( 'NONE',  ( -2.594671182134835163, -9.923034775318452461, 2.580184533305832861 ) ) ;
#16446 = CARTESIAN_POINT ( 'NONE',  ( 12.24655858231679595, -21.94931252712234127, 4.499999999999999112 ) ) ;
#16447 = CARTESIAN_POINT ( 'NONE',  ( 8.222191417683175629, -20.27099543870833998, 4.275561207030583510 ) ) ;
#16448 = CARTESIAN_POINT ( 'NONE',  ( -10.09030858231679595, -21.63647391050454871, 2.479004561291657804 ) ) ;
#16449 = VERTEX_POINT ( 'NONE', #15354 ) ;
#16450 = CARTESIAN_POINT ( 'NONE',  ( 13.07148796623841847, 1.547642295024179493, 6.704787912489258872 ) ) ;
#16451 = CARTESIAN_POINT ( 'NONE',  ( 12.62499999998404299, -19.49999999996810729, 2.793053905886972998 ) ) ;
#16452 = CARTESIAN_POINT ( 'NONE',  ( -12.90166454282617536, -19.87494034644570107, 3.513414777791785681 ) ) ;
#16453 = ORIENTED_EDGE ( 'NONE', *, *, #11065, .F. ) ;
#16454 = EDGE_CURVE ( 'NONE', #8626, #1180, #9186, .T. ) ;
#16455 = EDGE_LOOP ( 'NONE', ( #300, #19064, #10123, #18735, #14906, #16302 ) ) ;
#16456 = LINE ( 'NONE', #11947, #19150 ) ;
#16457 = AXIS2_PLACEMENT_3D ( 'NONE', #4616, #1390, #7772 ) ;
#16458 = CARTESIAN_POINT ( 'NONE',  ( -16.62779268661489951, 0.000000000000000000, 1.000000000000000000 ) ) ;
#16459 = FACE_OUTER_BOUND ( 'NONE', #1970, .T. ) ;
#16460 = DIRECTION ( 'NONE',  ( -0.000000000000000000, -0.000000000000000000, -1.000000000000000000 ) ) ;
#16461 = CARTESIAN_POINT ( 'NONE',  ( 1.710927537542899612, -9.866086492083725901, 2.372944093759576933 ) ) ;
#16462 = CARTESIAN_POINT ( 'NONE',  ( -13.49999999999998401, -24.49999999999999289, 1.000000000000000000 ) ) ;
#16463 = CARTESIAN_POINT ( 'NONE',  ( 14.50000000000000000, -23.00000000000001421, 4.000000000000000000 ) ) ;
#16464 = AXIS2_PLACEMENT_3D ( 'NONE', #18293, #18405, #3858 ) ;
#16465 = CARTESIAN_POINT ( 'NONE',  ( 0.000000000000000000, 16.00000000000000000, 1.000000000000000000 ) ) ;
#16466 = CARTESIAN_POINT ( 'NONE',  ( -1.904508877737772998, -9.138371295333994837, 2.378667276417936627 ) ) ;
#16467 = CARTESIAN_POINT ( 'NONE',  ( -6.059058582316793284, -20.72672167713054137, 4.701595411283463477 ) ) ;
#16468 = CARTESIAN_POINT ( 'NONE',  ( -3.257364212367626966, -9.501732542047829355, 2.664600686199549706 ) ) ;
#16469 = VERTEX_POINT ( 'NONE', #17132 ) ;
#16470 = CARTESIAN_POINT ( 'NONE',  ( -13.37847682517167947, -19.32442032882675775, 4.733786629989340078 ) ) ;
#16471 = CARTESIAN_POINT ( 'NONE',  ( -10.18405858231679417, -20.79840458871652942, 2.226721677130544030 ) ) ;
#16472 = VECTOR ( 'NONE', #19152, 1000.000000000000000 ) ;
#16473 = CARTESIAN_POINT ( 'NONE',  ( -5.503441417683176518, -22.05068747287765873, 5.250000000000000888 ) ) ;
#16474 = VERTEX_POINT ( 'NONE', #15459 ) ;
#16475 = CARTESIAN_POINT ( 'NONE',  ( 13.84501474873290938, 4.235744811019327649, 4.974109985360144037 ) ) ;
#16476 = DIRECTION ( 'NONE',  ( 1.000000000000000000, 0.000000000000000000, 0.000000000000000000 ) ) ;
#16477 = ORIENTED_EDGE ( 'NONE', *, *, #19502, .F. ) ;
#16478 = ORIENTED_EDGE ( 'NONE', *, *, #16019, .T. ) ;
#16479 = EDGE_CURVE ( 'NONE', #7462, #19218, #20081, .T. ) ;
#16480 = DIRECTION ( 'NONE',  ( 0.000000000000000000, -1.000000000000000000, 0.000000000000000000 ) ) ;
#16481 = ORIENTED_EDGE ( 'NONE', *, *, #9559, .F. ) ;
#16482 = DIRECTION ( 'NONE',  ( 1.000000000000000000, 0.000000000000000000, 0.000000000000000000 ) ) ;
#16483 = EDGE_LOOP ( 'NONE', ( #2153, #5841, #1306, #18080 ) ) ;
#16484 = CARTESIAN_POINT ( 'NONE',  ( 4.190941417683176518, -23.27327832286946219, 4.701595411283453707 ) ) ;
#16485 = DIRECTION ( 'NONE',  ( -1.000000000000000000, 0.000000000000000000, 0.000000000000000000 ) ) ;
#16486 = DIRECTION ( 'NONE',  ( -1.000000000000000000, 0.000000000000000000, 0.000000000000000000 ) ) ;
#16487 = CARTESIAN_POINT ( 'NONE',  ( 2.875042468481914248, -11.91375063635796039, 3.091440134965714126 ) ) ;
#16488 = CARTESIAN_POINT ( 'NONE',  ( -4.934058582316793284, -23.20159541128345992, 4.773278322869455970 ) ) ;
#16489 = CARTESIAN_POINT ( 'NONE',  ( 13.90411326029870409, 5.720219645086723759, 5.230514352905474063 ) ) ;
#16490 = DIRECTION ( 'NONE',  ( 5.204170427930411817E-15, -1.000000000000000000, 0.000000000000000000 ) ) ;
#16491 = CARTESIAN_POINT ( 'NONE',  ( 7.378441417683176518, -23.74999999999999645, 3.449312527122335492 ) ) ;
#16492 = DIRECTION ( 'NONE',  ( 0.000000000000000000, -1.000000000000000000, 0.000000000000000000 ) ) ;
#16493 = CARTESIAN_POINT ( 'NONE',  ( -6.534691417683177406, -20.97900456129164581, 3.136473910504570917 ) ) ;
#16494 = CARTESIAN_POINT ( 'NONE',  ( -8.871558582316795949, -19.49999999999998934, 3.449312527122348371 ) ) ;
#16495 = VERTEX_POINT ( 'NONE', #18606 ) ;
#16496 = CARTESIAN_POINT ( 'NONE',  ( 12.83635126708105823, -9.576761012430582198, 5.715524842913705328 ) ) ;
#16497 = CARTESIAN_POINT ( 'NONE',  ( -12.64195242771744709, -19.39390240027112000, 5.496549442168085164 ) ) ;
#16498 = ORIENTED_EDGE ( 'NONE', *, *, #8574, .T. ) ;
#16499 = PLANE ( 'NONE',  #5622 ) ;
#16500 = CARTESIAN_POINT ( 'NONE',  ( -14.49999999999999645, -22.99999999999998579, 1.000000000000000000 ) ) ;
#16501 = ORIENTED_EDGE ( 'NONE', *, *, #14375, .T. ) ;
#16502 = VERTEX_POINT ( 'NONE', #12317 ) ;
#16503 = EDGE_CURVE ( 'NONE', #16571, #15008, #20501, .T. ) ;
#16504 = CARTESIAN_POINT ( 'NONE',  ( -7.499999999999999112, -18.49999999999999645, 4.000000000000000000 ) ) ;
#16505 = ORIENTED_EDGE ( 'NONE', *, *, #3355, .T. ) ;
#16506 = DIRECTION ( 'NONE',  ( 0.000000000000000000, 0.000000000000000000, 1.000000000000000000 ) ) ;
#16507 = CARTESIAN_POINT ( 'NONE',  ( 13.10756170493883310, 4.119366099410778581, 6.001761809183453700 ) ) ;
#16508 = ADVANCED_FACE ( 'NONE', ( #2593 ), #20286, .T. ) ;
#16509 = CARTESIAN_POINT ( 'NONE',  ( -1.852280067228949445, -9.126254559850970338, 1.625555456689752321 ) ) ;
#16510 = DIRECTION ( 'NONE',  ( 1.000000000000000000, 0.000000000000000000, -0.000000000000000000 ) ) ;
#16511 = PLANE ( 'NONE',  #16464 ) ;
#16512 = EDGE_CURVE ( 'NONE', #9049, #10249, #5747, .T. ) ;
#16513 = CARTESIAN_POINT ( 'NONE',  ( 12.62888984277510218, -20.05356293986039873, 5.111704976569332537 ) ) ;
#16514 = DIRECTION ( 'NONE',  ( 0.000000000000000000, -1.000000000000000000, 0.000000000000000000 ) ) ;
#16515 = CARTESIAN_POINT ( 'NONE',  ( 11.87155858231679595, -19.49999999999998934, 3.449312527122348371 ) ) ;
#16516 = CARTESIAN_POINT ( 'NONE',  ( -12.62562019941893432, -20.21867992933967173, 4.757612834768309540 ) ) ;
#16517 = CARTESIAN_POINT ( 'NONE',  ( -4.753441417683176518, -21.94931252712233061, 0.9999999999999978906 ) ) ;
#16518 = FACE_OUTER_BOUND ( 'NONE', #6119, .T. ) ;
#16519 = CARTESIAN_POINT ( 'NONE',  ( 13.00209451496117374, 0.000000000000000000, 1.000000000000000000 ) ) ;
#16520 = CARTESIAN_POINT ( 'NONE',  ( 10.27780858231679595, -21.02099543870833998, 3.035098964749253003 ) ) ;
#16521 = CARTESIAN_POINT ( 'NONE',  ( -7.499999999999999112, -25.49999999999999645, 6.500000000000000888 ) ) ;
#16522 = ORIENTED_EDGE ( 'NONE', *, *, #7502, .F. ) ;
#16523 = ORIENTED_EDGE ( 'NONE', *, *, #13568, .T. ) ;
#16524 = CARTESIAN_POINT ( 'NONE',  ( 13.37499999999998401, -20.99999999999998934, 2.439580858552613751 ) ) ;
#16525 = DIRECTION ( 'NONE',  ( 0.000000000000000000, -0.000000000000000000, 1.000000000000000000 ) ) ;
#16526 = ORIENTED_EDGE ( 'NONE', *, *, #18891, .F. ) ;
#16527 = EDGE_CURVE ( 'NONE', #1939, #8463, #5730, .T. ) ;
#16528 = DIRECTION ( 'NONE',  ( 0.000000000000000000, 0.000000000000000000, 1.000000000000000000 ) ) ;
#16529 = DIRECTION ( 'NONE',  ( -1.000000000000000000, 0.000000000000000000, 0.000000000000000000 ) ) ;
#16530 = CARTESIAN_POINT ( 'NONE',  ( 23.60856191738414012, 9.000000000000001776, 0.000000000000000000 ) ) ;
#16531 = CARTESIAN_POINT ( 'NONE',  ( 13.37499999999998224, -20.25000000000006395, 4.416666666666681174 ) ) ;
#16532 = PLANE ( 'NONE',  #8530 ) ;
#16533 = CARTESIAN_POINT ( 'NONE',  ( 1.548630333695928618, -8.364917468222230923, 2.372643865078341019 ) ) ;
#16534 = DIRECTION ( 'NONE',  ( 0.000000000000000000, 1.000000000000000000, -0.000000000000000000 ) ) ;
#16535 = VECTOR ( 'NONE', #4597, 1000.000000000000000 ) ;
#16536 = CARTESIAN_POINT ( 'NONE',  ( -12.89855869007488209, -5.685286151195387383, 5.049178440009032265 ) ) ;
#16537 = CARTESIAN_POINT ( 'NONE',  ( 7.746558582316794173, -21.94931252712234482, 5.250000000000000888 ) ) ;
#16538 = PLANE ( 'NONE',  #18757 ) ;
#16539 = CARTESIAN_POINT ( 'NONE',  ( 13.10557919622060652, 4.019249409169220577, 6.007898877577752650 ) ) ;
#16540 = DIRECTION ( 'NONE',  ( 0.000000000000000000, 0.000000000000000000, 1.000000000000000000 ) ) ;
#16541 = CARTESIAN_POINT ( 'NONE',  ( 9.809058582316795949, -22.74294823697954016, 2.828734674606448785 ) ) ;
#16542 = CARTESIAN_POINT ( 'NONE',  ( 7.940941417683176518, -20.72672167713052715, 2.298404588716546293 ) ) ;
#16543 = CARTESIAN_POINT ( 'NONE',  ( -10.46530858231679417, -20.22900456129164937, 4.174186261275266929 ) ) ;
#16544 = ORIENTED_EDGE ( 'NONE', *, *, #11586, .T. ) ;
#16545 = CARTESIAN_POINT ( 'NONE',  ( 12.65986935584910000, -19.23909752961862907, 6.257782094979345899 ) ) ;
#16546 = CARTESIAN_POINT ( 'NONE',  ( 12.63298722613685676, -19.09664508008815531, 4.760766981674283471 ) ) ;
#16547 = DIRECTION ( 'NONE',  ( -1.000000000000000000, 0.000000000000000000, 0.000000000000000000 ) ) ;
#16548 = ORIENTED_EDGE ( 'NONE', *, *, #18430, .T. ) ;
#16549 = EDGE_CURVE ( 'NONE', #6959, #17483, #8980, .T. ) ;
#16550 = ORIENTED_EDGE ( 'NONE', *, *, #20048, .T. ) ;
#16551 = EDGE_CURVE ( 'NONE', #14519, #4780, #13673, .T. ) ;
#16552 = CARTESIAN_POINT ( 'NONE',  ( -26.04469207716615031, 9.000000000000001776, 1.000000000000000000 ) ) ;
#16553 = CARTESIAN_POINT ( 'NONE',  ( 10.93924542913430820, 10.00000000000000000, 0.000000000000000000 ) ) ;
#16554 = CARTESIAN_POINT ( 'NONE',  ( -26.04469207716614321, -2.255140518769849223E-14, 1.000000000000000000 ) ) ;
#16555 = CARTESIAN_POINT ( 'NONE',  ( -3.984239023773644028, -21.55980365857980630, 5.395836504137947465 ) ) ;
#16556 = CARTESIAN_POINT ( 'NONE',  ( 2.109407804498405703, -9.207748739546751438, 2.396484790045401603 ) ) ;
#16557 = DIRECTION ( 'NONE',  ( 0.000000000000000000, 0.9919684228235026158, 0.1264857625231113336 ) ) ;
#16558 = CARTESIAN_POINT ( 'NONE',  ( 11.00000000000000000, -23.70993649053891517, 5.466506350946108483 ) ) ;
#16559 = CARTESIAN_POINT ( 'NONE',  ( 13.18792642815267335, -20.57543385444909845, 3.474652748137723179 ) ) ;
#16560 = CARTESIAN_POINT ( 'NONE',  ( -22.06633994409548194, 0.000000000000000000, 1.000000000000000000 ) ) ;
#16561 = CARTESIAN_POINT ( 'NONE',  ( -7.934058582316792396, -23.20159541128345992, 4.773278322869455970 ) ) ;
#16562 = CARTESIAN_POINT ( 'NONE',  ( -3.365018999794965548, -10.14078633184679923, 2.828722465802024910 ) ) ;
#16563 = ORIENTED_EDGE ( 'NONE', *, *, #11662, .T. ) ;
#16564 = CARTESIAN_POINT ( 'NONE',  ( -13.37499999999998401, -19.49999999999998934, 3.146526952850934755 ) ) ;
#16565 = CARTESIAN_POINT ( 'NONE',  ( -6.902808582316793284, -22.77556120703056308, 1.770995438708339975 ) ) ;
#16566 = CARTESIAN_POINT ( 'NONE',  ( -6.628441417683176518, -20.24999999999999289, 3.550687472877664952 ) ) ;
#16567 = EDGE_LOOP ( 'NONE', ( #14927, #7656, #13540, #17553 ) ) ;
#16568 = CARTESIAN_POINT ( 'NONE',  ( 13.41341218697771609, -18.31018455762212227, 5.513179699623425023 ) ) ;
#16569 = DIRECTION ( 'NONE',  ( 1.000000000000000000, 0.000000000000000000, 0.000000000000000000 ) ) ;
#16570 = ORIENTED_EDGE ( 'NONE', *, *, #20354, .T. ) ;
#16571 = VERTEX_POINT ( 'NONE', #6157 ) ;
#16572 = LINE ( 'NONE', #2249, #696 ) ;
#16573 = ORIENTED_EDGE ( 'NONE', *, *, #4910, .T. ) ;
#16574 = CARTESIAN_POINT ( 'NONE',  ( -13.37327929115833491, -20.24999999560066399, 3.449077790995343840 ) ) ;
#16575 = ORIENTED_EDGE ( 'NONE', *, *, #17670, .F. ) ;
#16576 = CARTESIAN_POINT ( 'NONE',  ( 7.565941417683176518, -23.20159541128344927, 2.226721677130534705 ) ) ;
#16577 = CARTESIAN_POINT ( 'NONE',  ( 27.44203811574919882, 0.000000000000000000, 1.000000000000000000 ) ) ;
#16578 = DIRECTION ( 'NONE',  ( -1.000000000000000000, 0.000000000000000000, 0.000000000000000000 ) ) ;
#16579 = CARTESIAN_POINT ( 'NONE',  ( 1.513434189748285696, -9.114917468222230923, 2.372643865078341019 ) ) ;
#16580 = CARTESIAN_POINT ( 'NONE',  ( -5.027808582316793284, -23.72900456129165292, 4.275561207030568411 ) ) ;
#16581 = EDGE_CURVE ( 'NONE', #12176, #17531, #7617, .T. ) ;
#16582 = CARTESIAN_POINT ( 'NONE',  ( 12.62527129584495000, -20.98629955982801576, 4.726243163759704657 ) ) ;
#16583 = DIRECTION ( 'NONE',  ( -1.000000000000000000, -2.312964634635731617E-15, 0.000000000000000000 ) ) ;
#16584 = CARTESIAN_POINT ( 'NONE',  ( 12.34719141768317741, -21.53509896474923835, 2.520995438708346192 ) ) ;
#16585 = CARTESIAN_POINT ( 'NONE',  ( -12.64511805349267526, -19.23403829861753422, 5.507852591554869726 ) ) ;
#16586 = CARTESIAN_POINT ( 'NONE',  ( -7.940941417683175629, -21.25705176302044208, 2.828734674606458555 ) ) ;
#16587 = CARTESIAN_POINT ( 'NONE',  ( -7.746558582316795949, -21.94931252712234127, 6.000000000000001776 ) ) ;
#16588 = ORIENTED_EDGE ( 'NONE', *, *, #13121, .F. ) ;
#16589 = CARTESIAN_POINT ( 'NONE',  ( 12.62500797102436678, -19.49959746326937093, 4.516621614626514791 ) ) ;
#16590 = CARTESIAN_POINT ( 'NONE',  ( -12.79798428357658047, -11.51429367935891790, 5.673858176248284479 ) ) ;
#16591 = VERTEX_POINT ( 'NONE', #12424 ) ;
#16592 = CARTESIAN_POINT ( 'NONE',  ( -6.313547257480587760, 0.000000000000000000, 1.000000000000000000 ) ) ;
#16593 = DIRECTION ( 'NONE',  ( 1.000000000000000000, 0.000000000000000000, -0.000000000000000000 ) ) ;
#16594 = VERTEX_POINT ( 'NONE', #12118 ) ;
#16595 = ORIENTED_EDGE ( 'NONE', *, *, #18999, .T. ) ;
#16596 = CARTESIAN_POINT ( 'NONE',  ( 12.81218474072258040, -19.92450197877212048, 3.525331579139530547 ) ) ;
#16597 = EDGE_LOOP ( 'NONE', ( #15118, #19061, #19631, #7080, #11496, #5414, #13847, #220 ) ) ;
#16598 = CARTESIAN_POINT ( 'NONE',  ( -0.000000000000000000, 10.00000000000000000, 0.000000000000000000 ) ) ;
#16599 = CARTESIAN_POINT ( 'NONE',  ( 12.65051119073526564, -18.96168486786632457, 5.513701926248478102 ) ) ;
#16600 = CARTESIAN_POINT ( 'NONE',  ( -2.762374231067749708, -9.968169115173667549, 1.841775933429679268 ) ) ;
#16601 = CARTESIAN_POINT ( 'NONE',  ( -24.87918902992234393, 0.000000000000000000, 1.000000000000000000 ) ) ;
#16602 = DIRECTION ( 'NONE',  ( 0.000000000000000000, 0.000000000000000000, 1.000000000000000000 ) ) ;
#16603 = DIRECTION ( 'NONE',  ( -0.000000000000000000, -0.000000000000000000, -1.000000000000000000 ) ) ;
#16604 = FACE_OUTER_BOUND ( 'NONE', #4856, .T. ) ;
#16605 = CARTESIAN_POINT ( 'NONE',  ( 5.684058582316795949, -20.26807450282662160, 1.696391591240633101 ) ) ;
#16606 = CARTESIAN_POINT ( 'NONE',  ( -13.09892531043291086, 3.683228176858501790, 6.000681092915118420 ) ) ;
#16607 = CARTESIAN_POINT ( 'NONE',  ( -6.628441417683177406, -19.49999999999998934, 3.550687472877664952 ) ) ;
#16608 = EDGE_CURVE ( 'NONE', #8195, #6243, #13985, .T. ) ;
#16609 = ORIENTED_EDGE ( 'NONE', *, *, #17838, .T. ) ;
#16610 = CARTESIAN_POINT ( 'NONE',  ( 4.999999999999998224, 0.000000000000000000, 9.999999999999998224 ) ) ;
#16611 = DIRECTION ( 'NONE',  ( 0.000000000000000000, 0.9919684228235026158, -0.1264857625231113336 ) ) ;
#16612 = CARTESIAN_POINT ( 'NONE',  ( -13.75871503850933841, -0.8723905552644914962, 5.888179699623941943 ) ) ;
#16613 = CARTESIAN_POINT ( 'NONE',  ( 8.590308582316797725, -21.63647391050454871, 2.479004561291657804 ) ) ;
#16614 = DIRECTION ( 'NONE',  ( 1.000000000000000000, -0.000000000000000000, 0.000000000000000000 ) ) ;
#16615 = ORIENTED_EDGE ( 'NONE', *, *, #19788, .T. ) ;
#16616 = ORIENTED_EDGE ( 'NONE', *, *, #7561, .T. ) ;
#16617 = EDGE_CURVE ( 'NONE', #5681, #13158, #18714, .T. ) ;
#16618 = CARTESIAN_POINT ( 'NONE',  ( 13.41820805991576826, -18.06799297425606454, 5.518388032956592859 ) ) ;
#16619 = EDGE_CURVE ( 'NONE', #18960, #5420, #1143, .T. ) ;
#16620 = LINE ( 'NONE', #10052, #9810 ) ;
#16621 =( NAMED_UNIT ( * ) SI_UNIT ( $, .STERADIAN. ) SOLID_ANGLE_UNIT ( ) );
#16622 = ORIENTED_EDGE ( 'NONE', *, *, #18885, .F. ) ;
#16623 = CARTESIAN_POINT ( 'NONE',  ( -9.805650798910056309, 0.000000000000000000, 0.000000000000000000 ) ) ;
#16624 = DIRECTION ( 'NONE',  ( -0.000000000000000000, -0.000000000000000000, -1.000000000000000000 ) ) ;
#16625 = AXIS2_PLACEMENT_3D ( 'NONE', #16702, #7097, #15140 ) ;
#16626 = DIRECTION ( 'NONE',  ( 1.000000000000000000, 0.000000000000000000, -0.000000000000000000 ) ) ;
#16627 = CARTESIAN_POINT ( 'NONE',  ( 13.37500000000002132, -20.24999999999450040, 3.833333333368183382 ) ) ;
#16628 = DIRECTION ( 'NONE',  ( -1.000000000000000000, 0.000000000000000000, 0.000000000000000000 ) ) ;
#16629 = CARTESIAN_POINT ( 'NONE',  ( 2.171407406650392780, -8.432416083433171394, 2.389978857884845986 ) ) ;
#16630 = CARTESIAN_POINT ( 'NONE',  ( -13.49999999999998401, -18.49999999999999645, 4.000000000000000000 ) ) ;
#16631 = CARTESIAN_POINT ( 'NONE',  ( -12.62499999999998401, -19.49999999999998934, 3.146526952850934755 ) ) ;
#16632 = CARTESIAN_POINT ( 'NONE',  ( 7.934058582316792396, -23.20159541128345992, 4.773278322869455970 ) ) ;
#16633 = CARTESIAN_POINT ( 'NONE',  ( 11.99999999999999822, -25.50000000000000355, 4.000000000000000000 ) ) ;
#16634 = CARTESIAN_POINT ( 'NONE',  ( 13.00900269284621302, -0.8578640112522492034, 5.903024842915844062 ) ) ;
#16635 = EDGE_CURVE ( 'NONE', #200, #17877, #4579, .T. ) ;
#16636 = AXIS2_PLACEMENT_3D ( 'NONE', #6979, #18070, #4047 ) ;
#16637 = FACE_OUTER_BOUND ( 'NONE', #16380, .T. ) ;
#16638 = CARTESIAN_POINT ( 'NONE',  ( 7.371558582316795949, -20.99999999999999645, 3.449312527122348371 ) ) ;
#16639 = CARTESIAN_POINT ( 'NONE',  ( 11.59719141768317563, -22.77556120703057729, 5.229004561291655584 ) ) ;
#16640 = CARTESIAN_POINT ( 'NONE',  ( -9.340308582316794173, -22.67418626127525982, 5.270995438708342640 ) ) ;
#16641 = ORIENTED_EDGE ( 'NONE', *, *, #9359, .F. ) ;
#16642 = CARTESIAN_POINT ( 'NONE',  ( 13.10745701327265778, 3.364079170269163921, 6.743850412489304169 ) ) ;
#16643 = ADVANCED_FACE ( 'NONE', ( #1036 ), #5849, .F. ) ;
#16644 = CARTESIAN_POINT ( 'NONE',  ( 12.64917329730235096, -18.27924848622803466, 4.778345106674467324 ) ) ;
#16645 = EDGE_CURVE ( 'NONE', #15085, #7740, #4268, .T. ) ;
#16646 = CARTESIAN_POINT ( 'NONE',  ( 0.000000000000000000, 11.64110105645932691, 10.00000000000000000 ) ) ;
#16647 = EDGE_LOOP ( 'NONE', ( #3723, #1875, #18569, #6511 ) ) ;
#16648 = ORIENTED_EDGE ( 'NONE', *, *, #520, .T. ) ;
#16649 = CARTESIAN_POINT ( 'NONE',  ( -13.49999999999998401, -24.47992105705875332, 12.00000000000000000 ) ) ;
#16650 = CIRCLE ( 'NONE', #7646, 2.999999999999999112 ) ;
#16651 = DIRECTION ( 'NONE',  ( 0.000000000000000000, 1.000000000000000000, -0.000000000000000000 ) ) ;
#16652 = AXIS2_PLACEMENT_3D ( 'NONE', #5380, #14890, #8622 ) ;
#16653 = VECTOR ( 'NONE', #18400, 1000.000000000000000 ) ;
#16654 = DIRECTION ( 'NONE',  ( 0.000000000000000000, 0.000000000000000000, -1.000000000000000000 ) ) ;
#16655 = CARTESIAN_POINT ( 'NONE',  ( -4.315753587183822404, -21.47141115243053378, 5.558207674221720573 ) ) ;
#16656 = CARTESIAN_POINT ( 'NONE',  ( 2.594671182134835163, -9.923034775318452461, 2.580184533305832861 ) ) ;
#16657 = DIRECTION ( 'NONE',  ( 0.000000000000000000, -0.000000000000000000, 1.000000000000000000 ) ) ;
#16658 = DIRECTION ( 'NONE',  ( -1.000000000000000000, -6.938893903907222067E-15, 0.000000000000000000 ) ) ;
#16659 = EDGE_CURVE ( 'NONE', #4928, #3941, #7728, .T. ) ;
#16660 = DIRECTION ( 'NONE',  ( 1.000000000000000000, 0.000000000000000000, 0.000000000000000000 ) ) ;
#16661 = CARTESIAN_POINT ( 'NONE',  ( -1.717920576997000737, -9.114924032904250240, 2.372645551019823884 ) ) ;
#16662 = CARTESIAN_POINT ( 'NONE',  ( -6.152808582316793284, -21.22443879296942626, 5.229004561291659137 ) ) ;
#16663 = CARTESIAN_POINT ( 'NONE',  ( -1.643076795806035717, -8.364903549957356077, 2.372640290589878909 ) ) ;
#16664 = VECTOR ( 'NONE', #19204, 1000.000000000000000 ) ;
#16665 = ORIENTED_EDGE ( 'NONE', *, *, #2817, .F. ) ;
#16666 = VECTOR ( 'NONE', #1754, 1000.000000000000000 ) ;
#16667 = CARTESIAN_POINT ( 'NONE',  ( -13.41806913471718588, -17.32500869677464550, 4.784333296715663764 ) ) ;
#16668 = CARTESIAN_POINT ( 'NONE',  ( -6.152808582316793284, -21.22443879296942626, 5.229004561291659137 ) ) ;
#16669 = CARTESIAN_POINT ( 'NONE',  ( 12.71530858231679417, -24.52099543870834708, 2.515153566944913432 ) ) ;
#16670 = CARTESIAN_POINT ( 'NONE',  ( -10.94094141768317741, -21.25705176302044208, 2.828734674606458555 ) ) ;
#16671 = VECTOR ( 'NONE', #3639, 1000.000000000000000 ) ;
#16672 = ORIENTED_EDGE ( 'NONE', *, *, #55, .T. ) ;
#16673 = CARTESIAN_POINT ( 'NONE',  ( 13.38450946332969771, -19.76977210184853462, 5.359796180098093998 ) ) ;
#16674 = DIRECTION ( 'NONE',  ( -0.000000000000000000, -0.000000000000000000, -1.000000000000000000 ) ) ;
#16675 = ORIENTED_EDGE ( 'NONE', *, *, #10818, .F. ) ;
#16676 = VERTEX_POINT ( 'NONE', #20597 ) ;
#16677 = LINE ( 'NONE', #7073, #6377 ) ;
#16678 = ORIENTED_EDGE ( 'NONE', *, *, #18688, .T. ) ;
#16679 = CARTESIAN_POINT ( 'NONE',  ( -13.37500000000002132, -20.24999999999450040, 3.833333333368183382 ) ) ;
#16680 = VECTOR ( 'NONE', #10622, 1000.000000000000000 ) ;
#16681 = ORIENTED_EDGE ( 'NONE', *, *, #7052, .T. ) ;
#16682 = CARTESIAN_POINT ( 'NONE',  ( 4.097191417683176518, -22.77556120703057729, 5.229004561291656472 ) ) ;
#16683 = DIRECTION ( 'NONE',  ( 1.000000000000000000, 0.000000000000000000, -0.000000000000000000 ) ) ;
#16684 = AXIS2_PLACEMENT_3D ( 'NONE', #9630, #17481, #11208 ) ;
#16685 = DIRECTION ( 'NONE',  ( 0.000000000000000000, 0.000000000000000000, 1.000000000000000000 ) ) ;
#16686 = CARTESIAN_POINT ( 'NONE',  ( 2.171407406650392780, -8.432416083433171394, 2.389978857884845986 ) ) ;
#16687 = CARTESIAN_POINT ( 'NONE',  ( -6.340308582316794173, -22.67418626127525982, 5.270995438708342640 ) ) ;
#16688 = VECTOR ( 'NONE', #1376, 1000.000000000000000 ) ;
#16689 = EDGE_CURVE ( 'NONE', #12925, #551, #4885, .T. ) ;
#16690 = CARTESIAN_POINT ( 'NONE',  ( 12.65816212372154403, -19.32531275206247301, 6.255900543948403225 ) ) ;
#16691 = CARTESIAN_POINT ( 'NONE',  ( -14.49999999999998579, -24.49999999999999289, 4.000000000000000000 ) ) ;
#16692 = EDGE_CURVE ( 'NONE', #16247, #3875, #17644, .T. ) ;
#16693 = CARTESIAN_POINT ( 'NONE',  ( 4.565941417683176518, -23.20159541128344927, 2.226721677130534705 ) ) ;
#16694 = FACE_OUTER_BOUND ( 'NONE', #5231, .T. ) ;
#16695 = CARTESIAN_POINT ( 'NONE',  ( -8.315941417683177406, -21.32873467460645145, 4.242948236979555254 ) ) ;
#16696 = CARTESIAN_POINT ( 'NONE',  ( -12.53469141768317741, -19.47900456129164581, 2.515153566944927199 ) ) ;
#16697 = VERTEX_POINT ( 'NONE', #19234 ) ;
#16698 = CARTESIAN_POINT ( 'NONE',  ( 12.62499999999998224, -19.49999999999998934, 4.291666666666699825 ) ) ;
#16699 = CARTESIAN_POINT ( 'NONE',  ( -13.10756170493883310, 4.119366099410778581, 6.001761809183453700 ) ) ;
#16700 = CIRCLE ( 'NONE', #17708, 10.00000000000000000 ) ;
#16701 = EDGE_LOOP ( 'NONE', ( #20409, #19327, #1466, #11007 ) ) ;
#16702 = CARTESIAN_POINT ( 'NONE',  ( 9.000000000000000000, -9.999999999999991118, 1.000000000000000000 ) ) ;
#16703 = DIRECTION ( 'NONE',  ( -0.8660254037844417052, 0.4999999999999948375, 0.000000000000000000 ) ) ;
#16704 =( GEOMETRIC_REPRESENTATION_CONTEXT ( 3 ) GLOBAL_UNCERTAINTY_ASSIGNED_CONTEXT ( ( #7769 ) ) GLOBAL_UNIT_ASSIGNED_CONTEXT ( ( #18732, #10981, #9305 ) ) REPRESENTATION_CONTEXT ( 'NONE', 'WORKASPACE' ) );
#16705 = ORIENTED_EDGE ( 'NONE', *, *, #18860, .F. ) ;
#16706 = ORIENTED_EDGE ( 'NONE', *, *, #8129, .F. ) ;
#16707 = EDGE_CURVE ( 'NONE', #11135, #13949, #9496, .T. ) ;
#16708 = AXIS2_PLACEMENT_3D ( 'NONE', #3780, #16529, #2205 ) ;
#16709 = ORIENTED_EDGE ( 'NONE', *, *, #6786, .T. ) ;
#16710 = DIRECTION ( 'NONE',  ( 1.000000000000000000, -1.156482317317871133E-15, 0.000000000000000000 ) ) ;
#16711 = CARTESIAN_POINT ( 'NONE',  ( -18.98630159782011262, 4.999999999999999112, 1.000000000000000000 ) ) ;
#16712 = CARTESIAN_POINT ( 'NONE',  ( -3.347120161770001268, -14.10934257735911146, 2.905312006771028077 ) ) ;
#16713 = LINE ( 'NONE', #8781, #10033 ) ;
#16714 = DIRECTION ( 'NONE',  ( -1.000000000000000000, 0.000000000000000000, 0.000000000000000000 ) ) ;
#16715 = DIRECTION ( 'NONE',  ( 0.000000000000000000, 1.000000000000000000, -0.000000000000000000 ) ) ;
#16716 = CARTESIAN_POINT ( 'NONE',  ( -7.559058582316794173, -20.72672167713054137, 4.701595411283463477 ) ) ;
#16717 = LINE ( 'NONE', #5749, #1007 ) ;
#16718 = AXIS2_PLACEMENT_3D ( 'NONE', #4201, #16853, #7242 ) ;
#16719 = CARTESIAN_POINT ( 'NONE',  ( 9.440941417683177406, -20.19639159124061933, 1.768074502826635586 ) ) ;
#16720 = CARTESIAN_POINT ( 'NONE',  ( -12.69247507894198712, -16.84250851341299082, 5.559274842915185033 ) ) ;
#16721 = VECTOR ( 'NONE', #1941, 1000.000000000000114 ) ;
#16722 = CARTESIAN_POINT ( 'NONE',  ( -4.378441417683176518, -24.50000000000000000, 3.449312527122335048 ) ) ;
#16723 = AXIS2_PLACEMENT_3D ( 'NONE', #12381, #18664, #7677 ) ;
#16724 = VECTOR ( 'NONE', #7236, 1000.000000000000000 ) ;
#16725 = ORIENTED_EDGE ( 'NONE', *, *, #795, .T. ) ;
#16726 = CARTESIAN_POINT ( 'NONE',  ( 10.65280858231679240, -21.22443879296942626, 5.229004561291659137 ) ) ;
#16727 = LINE ( 'NONE', #17037, #11414 ) ;
#16728 = CARTESIAN_POINT ( 'NONE',  ( -13.88684657106908205, 4.848251838987907014, 6.535242036940271504 ) ) ;
#16729 = VECTOR ( 'NONE', #3597, 1000.000000000000000 ) ;
#16730 = CARTESIAN_POINT ( 'NONE',  ( 13.37155858231679417, -20.24999999999999289, 3.449312527122348371 ) ) ;
#16731 = CARTESIAN_POINT ( 'NONE',  ( -14.49999999999998579, -25.49999999999999645, 4.000000000000000000 ) ) ;
#16732 = EDGE_LOOP ( 'NONE', ( #20281, #16251, #10747, #19532 ) ) ;
#16733 = EDGE_LOOP ( 'NONE', ( #17579, #11969, #11179, #768, #3336, #7176 ) ) ;
#16734 = CARTESIAN_POINT ( 'NONE',  ( 13.85163507668220539, 3.820071372449974412, 5.989091157956555556 ) ) ;
#16735 = LINE ( 'NONE', #11515, #15106 ) ;
#16736 = EDGE_LOOP ( 'NONE', ( #3848, #17193, #10700, #18368 ) ) ;
#16737 = EDGE_CURVE ( 'NONE', #8228, #7887, #20335, .T. ) ;
#16738 = LINE ( 'NONE', #945, #7121 ) ;
#16739 = LINE ( 'NONE', #10474, #9046 ) ;
#16740 = AXIS2_PLACEMENT_3D ( 'NONE', #16772, #9037, #14041 ) ;
#16741 = ADVANCED_FACE ( 'NONE', ( #13145 ), #11879, .T. ) ;
#16742 = CARTESIAN_POINT ( 'NONE',  ( 13.39722611581222189, -19.12758115148224647, 5.495601574623241170 ) ) ;
#16743 = AXIS2_PLACEMENT_3D ( 'NONE', #11360, #16181, #17749 ) ;
#16744 = DIRECTION ( 'NONE',  ( 0.000000000000000000, 1.000000000000000000, 0.000000000000000000 ) ) ;
#16745 = CARTESIAN_POINT ( 'NONE',  ( 1.728780693989796724, -8.364929292255887106, 2.372646901726390478 ) ) ;
#16746 = LINE ( 'NONE', #18635, #19090 ) ;
#16747 = CARTESIAN_POINT ( 'NONE',  ( -12.63298722613685676, -19.09664508008815531, 4.760766981674283471 ) ) ;
#16748 =( NAMED_UNIT ( * ) PLANE_ANGLE_UNIT ( ) SI_UNIT ( $, .RADIAN. ) );
#16749 = CARTESIAN_POINT ( 'NONE',  ( 11.59030858231679417, -21.32581373872472597, 1.729004561291657582 ) ) ;
#16750 = CARTESIAN_POINT ( 'NONE',  ( -13.37500000000002132, -21.00000000000274269, 4.083333333315724012 ) ) ;
#16751 = CARTESIAN_POINT ( 'NONE',  ( 3.999999999999999112, -7.500000000000047073, 2.000000000000000000 ) ) ;
#16752 = CARTESIAN_POINT ( 'NONE',  ( 6.152808582316795949, -21.53509896474924901, 4.479004561291659137 ) ) ;
#16753 = VECTOR ( 'NONE', #9835, 1000.000000000000000 ) ;
#16754 = CARTESIAN_POINT ( 'NONE',  ( 11.59719141768317741, -22.46490103525075810, 4.479004561291653808 ) ) ;
#16755 = CARTESIAN_POINT ( 'NONE',  ( -10.09030858231679595, -21.32581373872472597, 1.729004561291657582 ) ) ;
#16756 = ORIENTED_EDGE ( 'NONE', *, *, #14537, .T. ) ;
#16757 = CARTESIAN_POINT ( 'NONE',  ( 12.65457057572495181, -19.50668592589112293, 6.238308001337955488 ) ) ;
#16758 = CARTESIAN_POINT ( 'NONE',  ( 13.08559773465513487, 3.760185600081874746, 5.252303440007609403 ) ) ;
#16759 = CARTESIAN_POINT ( 'NONE',  ( 12.25209451496117197, 10.00000000000000000, 0.000000000000000000 ) ) ;
#16760 = ORIENTED_EDGE ( 'NONE', *, *, #5239, .F. ) ;
#16761 = ORIENTED_EDGE ( 'NONE', *, *, #18479, .F. ) ;
#16762 = DIRECTION ( 'NONE',  ( 0.000000000000000000, 0.000000000000000000, 1.000000000000000000 ) ) ;
#16763 = EDGE_CURVE ( 'NONE', #13679, #3772, #18270, .T. ) ;
#16764 = FACE_OUTER_BOUND ( 'NONE', #3465, .T. ) ;
#16765 = CARTESIAN_POINT ( 'NONE',  ( -1.437849085826860884, 16.00000000000000000, 1.000000000000000000 ) ) ;
#16766 = CIRCLE ( 'NONE', #4415, 0.5000000000000000000 ) ;
#16767 = ADVANCED_FACE ( 'NONE', ( #3932 ), #17955, .T. ) ;
#16768 = CARTESIAN_POINT ( 'NONE',  ( 5.381197846483058989, -14.00000000000000000, 2.000000000000000000 ) ) ;
#16769 = CARTESIAN_POINT ( 'NONE',  ( 1.548630333695928618, -9.864917468222230923, 2.372643865078341019 ) ) ;
#16770 = DIRECTION ( 'NONE',  ( 0.000000000000000000, 1.000000000000000000, 0.000000000000000000 ) ) ;
#16771 = EDGE_CURVE ( 'NONE', #13229, #12054, #8449, .T. ) ;
#16772 = CARTESIAN_POINT ( 'NONE',  ( -12.50209451496117197, 11.64110105645932691, 10.00000000000000000 ) ) ;
#16773 = CARTESIAN_POINT ( 'NONE',  ( -2.203959450683124377, -9.262433282444222371, 2.410528873095051594 ) ) ;
#16774 = CARTESIAN_POINT ( 'NONE',  ( -9.715308582316794173, -23.77099543870833998, 2.825813738724734847 ) ) ;
#16775 = CARTESIAN_POINT ( 'NONE',  ( -2.747777887823422471, -9.906471667804277459, 1.825930796414880763 ) ) ;
#16776 = EDGE_LOOP ( 'NONE', ( #1711, #19629, #2748, #480 ) ) ;
#16777 = CARTESIAN_POINT ( 'NONE',  ( -13.09560264576187905, 4.265433610975056133, 4.666666666666618113 ) ) ;
#16778 = VECTOR ( 'NONE', #3668, 1000.000000000000000 ) ;
#16779 = CARTESIAN_POINT ( 'NONE',  ( -9.434058582316794173, -23.20159541128345992, 4.773278322869455970 ) ) ;
#16780 = CARTESIAN_POINT ( 'NONE',  ( 9.340308582316795949, -22.98484643305508612, 6.020995438708344416 ) ) ;
#16781 = CARTESIAN_POINT ( 'NONE',  ( -11.22219141768317741, -21.02099543870834353, 3.964901035250761208 ) ) ;
#16782 = ORIENTED_EDGE ( 'NONE', *, *, #11787, .F. ) ;
#16783 = CARTESIAN_POINT ( 'NONE',  ( 13.85723511636018301, 4.102873376188801657, 5.986996695041598926 ) ) ;
#16784 = CARTESIAN_POINT ( 'NONE',  ( 0.000000000000000000, 9.000000000000001776, 1.000000000000000000 ) ) ;
#16785 = ORIENTED_EDGE ( 'NONE', *, *, #9030, .F. ) ;
#16786 = ORIENTED_EDGE ( 'NONE', *, *, #3216, .T. ) ;
#16787 = VECTOR ( 'NONE', #14550, 1000.000000000000000 ) ;
#16788 = CARTESIAN_POINT ( 'NONE',  ( 23.31633994409548549, 11.64110105645932691, 0.000000000000000000 ) ) ;
#16789 = ORIENTED_EDGE ( 'NONE', *, *, #3761, .F. ) ;
#16790 = CARTESIAN_POINT ( 'NONE',  ( -9.000000000000000000, -9.999999999999992895, 1.000000000000000000 ) ) ;
#16791 = ADVANCED_FACE ( 'NONE', ( #14817 ), #491, .T. ) ;
#16792 = EDGE_LOOP ( 'NONE', ( #10613, #11541, #6535, #4852, #12103, #12268, #11712, #19580, #11609, #9791 ) ) ;
#16793 = CARTESIAN_POINT ( 'NONE',  ( 7.499999999999999112, -25.49999999999999645, 6.500000000000000888 ) ) ;
#16794 = CYLINDRICAL_SURFACE ( 'NONE', #11010, 10.00000000000000000 ) ;
#16795 = CARTESIAN_POINT ( 'NONE',  ( -13.50000000000000178, 0.000000000000000000, 2.000000000000000000 ) ) ;
#16796 = CARTESIAN_POINT ( 'NONE',  ( 0.9854920305337622199, -8.364917468222230923, 2.372643865078341019 ) ) ;
#16797 = CARTESIAN_POINT ( 'NONE',  ( 27.00000000000000000, 0.000000000000000000, 1.000000000000000000 ) ) ;
#16798 = AXIS2_PLACEMENT_3D ( 'NONE', #2301, #10254, #5141 ) ;
#16799 = CARTESIAN_POINT ( 'NONE',  ( 13.86833701876684088, 3.913519447696059750, 6.741146579470268740 ) ) ;
#16800 = LINE ( 'NONE', #2469, #14967 ) ;
#16801 = CARTESIAN_POINT ( 'NONE',  ( 11.22219141768317741, -21.02099543870834353, 3.964901035250761208 ) ) ;
#16802 = CARTESIAN_POINT ( 'NONE',  ( -0.000000000000000000, 11.64110105645932691, 0.000000000000000000 ) ) ;
#16803 = EDGE_CURVE ( 'NONE', #381, #3752, #10845, .T. ) ;
#16804 = CARTESIAN_POINT ( 'NONE',  ( -6.909691417683176518, -21.63647391050456648, 4.520995438708348857 ) ) ;
#16805 = CARTESIAN_POINT ( 'NONE',  ( -9.347191417683177406, -20.91377862118959285, 1.020995438708345082 ) ) ;
#16806 = ORIENTED_EDGE ( 'NONE', *, *, #18048, .T. ) ;
#16807 = CARTESIAN_POINT ( 'NONE',  ( 12.62691554569741648, -19.40326494227377907, 4.703927990036796736 ) ) ;
#16808 = CARTESIAN_POINT ( 'NONE',  ( -13.10557919622060652, 4.019249409169220577, 6.007898877577752650 ) ) ;
#16809 = ORIENTED_EDGE ( 'NONE', *, *, #796, .F. ) ;
#16810 = DIRECTION ( 'NONE',  ( 0.000000000000000000, 0.000000000000000000, -1.000000000000000000 ) ) ;
#16811 = PLANE ( 'NONE',  #13649 ) ;
#16812 = VECTOR ( 'NONE', #7943, 1000.000000000000000 ) ;
#16813 = ORIENTED_EDGE ( 'NONE', *, *, #17219, .F. ) ;
#16814 = SHAPE_DEFINITION_REPRESENTATION ( #2006, #14706 ) ;
#16815 = ORIENTED_EDGE ( 'NONE', *, *, #3188, .F. ) ;
#16816 = EDGE_CURVE ( 'NONE', #9078, #1461, #5722, .T. ) ;
#16817 = EDGE_CURVE ( 'NONE', #10698, #8256, #15634, .T. ) ;
#16818 = ORIENTED_EDGE ( 'NONE', *, *, #6030, .T. ) ;
#16819 = CARTESIAN_POINT ( 'NONE',  ( -20.00349085826861995, 11.64110105645932691, 0.000000000000000000 ) ) ;
#16820 = LINE ( 'NONE', #19971, #2594 ) ;
#16821 = EDGE_CURVE ( 'NONE', #9770, #962, #2885, .T. ) ;
#16822 = CARTESIAN_POINT ( 'NONE',  ( -2.787023586469211001, -10.13267000451481614, 1.884023048047904103 ) ) ;
#16823 = FACE_OUTER_BOUND ( 'NONE', #18335, .T. ) ;
#16824 = DIRECTION ( 'NONE',  ( -1.000000000000000000, 0.000000000000000000, 0.000000000000000000 ) ) ;
#16825 = DIRECTION ( 'NONE',  ( -0.000000000000000000, -0.000000000000000000, -1.000000000000000000 ) ) ;
#16826 = CARTESIAN_POINT ( 'NONE',  ( 10.84719141768317741, -20.91377862118959285, 1.020995438708345082 ) ) ;
#16827 = CARTESIAN_POINT ( 'NONE',  ( -13.08094078691552831, 2.775009739235173356, 5.981149842915306714 ) ) ;
#16828 = CARTESIAN_POINT ( 'NONE',  ( -5.690941417683177406, -23.80360840875937001, 5.231925497173365081 ) ) ;
#16829 = ORIENTED_EDGE ( 'NONE', *, *, #18241, .T. ) ;
#16830 = FACE_OUTER_BOUND ( 'NONE', #12519, .T. ) ;
#16831 = LINE ( 'NONE', #12531, #8093 ) ;
#16832 = CARTESIAN_POINT ( 'NONE',  ( -13.89075858682503650, 5.045808634669852744, 6.406973581600956535 ) ) ;
#16833 = CARTESIAN_POINT ( 'NONE',  ( 10.27780858231679417, -20.27099543870833642, 2.724438792969431589 ) ) ;
#16834 = DIRECTION ( 'NONE',  ( 1.000000000000000000, 0.000000000000000000, 0.000000000000000000 ) ) ;
#16835 = ORIENTED_EDGE ( 'NONE', *, *, #18173, .F. ) ;
#16836 = ORIENTED_EDGE ( 'NONE', *, *, #5174, .F. ) ;
#16837 = CARTESIAN_POINT ( 'NONE',  ( 13.70116456325478893, -3.778689555664588973, 5.825679699621801433 ) ) ;
#16838 = PLANE ( 'NONE',  #13957 ) ;
#16839 = SURFACE_STYLE_USAGE ( .BOTH. , #18310 ) ;
#16840 = ORIENTED_EDGE ( 'NONE', *, *, #10564, .T. ) ;
#16841 = CARTESIAN_POINT ( 'NONE',  ( -5.933390479346035029, 4.999999999999999112, 1.000000000000000000 ) ) ;
#16842 = LINE ( 'NONE', #10364, #17382 ) ;
#16843 = CARTESIAN_POINT ( 'NONE',  ( 0.000000000000000000, 11.64110105645932691, 10.00000000000000000 ) ) ;
#16844 = CARTESIAN_POINT ( 'NONE',  ( 13.87470602645761986, 4.985154336109792972, 4.333333333333379223 ) ) ;
#16845 =( BOUNDED_CURVE ( )  B_SPLINE_CURVE ( 2, ( #17064, #4417, #15699, #1480, #14222, #7554, #1275, #20534, #10900, #20630, #6187, #2744, #14327, #15591, #12357, #9528, #6283, #18751, #12657, #18953, #4608, #9124, #10801, #2845, #17371, #7954, #17478, #15900, #7655, #14751, #120, #11205, #12968, #8271, #3663, #17578, #1994, #3252, #17892, #6505, #14543, #17686, #6400, #14850, #11299, #3357, #19575, #4824, #8073, #3459, #8481, #1891, #13077, #9624, #14641, #16121, #19479, #429, #16010, #8175, #11407, #12867, #1687, #323, #16224, #6601, #9939, #4921, #19372, #19269, #17793, #14438, #6708, #5132, #11511, #5027, #5229, #215, #9736, #12767, #3559, #9837, #16318, #8379, #1788, #6808, #13176, #11607, #17992, #10047, #19170, #16421, #2098, #14947, #12129 ),
 .UNSPECIFIED., .F., .F. ) 
 B_SPLINE_CURVE_WITH_KNOTS ( ( 3, 2, 2, 2, 2, 2, 2, 2, 2, 2, 2, 2, 2, 2, 2, 2, 2, 2, 2, 2, 2, 2, 2, 2, 2, 2, 2, 2, 2, 2, 2, 2, 2, 2, 2, 2, 2, 2, 2, 2, 2, 2, 2, 2, 2, 2, 2, 3 ),
 ( 0.000000000000000000, 0.02083333333333333218, 0.04166666666666666435, 0.06250000000000000000, 0.08333333333333332871, 0.1041666666666666713, 0.1250000000000000000, 0.1458333333333333426, 0.1666666666666666574, 0.1875000000000000000, 0.2083333333333333426, 0.2291666666666666574, 0.2500000000000000000, 0.2708333333333333148, 0.2916666666666666852, 0.3124999999999999445, 0.3333333333333333148, 0.3541666666666666852, 0.3750000000000000000, 0.3958333333333333148, 0.4166666666666666852, 0.4375000000000000555, 0.4583333333333333148, 0.4791666666666666852, 0.5000000000000000000, 0.5208333333333333703, 0.5416666666666666297, 0.5625000000000000000, 0.5833333333333333703, 0.6041666666666666297, 0.6249999999999998890, 0.6458333333333333703, 0.6666666666666666297, 0.6875000000000000000, 0.7083333333333333703, 0.7291666666666666297, 0.7500000000000000000, 0.7708333333333333703, 0.7916666666666666297, 0.8125000000000000000, 0.8333333333333333703, 0.8541666666666666297, 0.8750000000000001110, 0.8958333333333333703, 0.9166666666666666297, 0.9375000000000000000, 0.9583333333333333703, 0.9650437087885355147 ),
 .UNSPECIFIED. ) 
 CURVE ( )  GEOMETRIC_REPRESENTATION_ITEM ( )  RATIONAL_B_SPLINE_CURVE ( ( 1.000000000000000000, 0.9238795325112867385, 1.000000000000000000, 0.9238795325112867385, 1.000000000000000000, 0.9238795325112867385, 1.000000000000000000, 0.9238795325112867385, 1.000000000000000000, 0.9238795325112867385, 1.000000000000000000, 0.9238795325112867385, 1.000000000000000000, 0.9238795325112867385, 1.000000000000000000, 0.9238795325112867385, 1.000000000000000000, 0.9238795325112867385, 1.000000000000000000, 0.9238795325112867385, 1.000000000000000000, 0.9238795325112867385, 1.000000000000000000, 0.9238795325112867385, 1.000000000000000000, 0.9238795325112867385, 1.000000000000000000, 0.9238795325112867385, 1.000000000000000000, 0.9238795325112867385, 1.000000000000000000, 0.9238795325112867385, 1.000000000000000000, 0.9238795325112867385, 1.000000000000000000, 0.9238795325112867385, 1.000000000000000000, 0.9238795325112867385, 1.000000000000000000, 0.9238795325112867385, 1.000000000000000000, 0.9238795325112867385, 1.000000000000000000, 0.9238795325112867385, 1.000000000000000000, 0.9238795325112867385, 1.000000000000000000, 0.9238795325112867385, 1.000000000000000000, 0.9238795325112867385, 1.000000000000000000, 0.9238795325112867385, 1.000000000000000000, 0.9238795325112867385, 1.000000000000000000, 0.9238795325112867385, 1.000000000000000000, 0.9238795325112867385, 1.000000000000000000, 0.9238795325112867385, 1.000000000000000000, 0.9238795325112867385, 1.000000000000000000, 0.9238795325112867385, 1.000000000000000000, 0.9238795325112867385, 1.000000000000000000, 0.9238795325112867385, 1.000000000000000000, 0.9238795325112867385, 1.000000000000000000, 0.9238795325112867385, 1.000000000000000000, 0.9238795325112867385, 1.000000000000000000, 0.9238795325112867385, 1.000000000000000000, 0.9238795325112867385, 1.000000000000000000, 0.9238795325112867385, 1.000000000000000000, 0.9238795325112867385, 1.000000000000000000, 0.9238795325112867385, 1.000000000000000000, 0.9238795325112867385, 1.000000000000000000, 0.9238795325112867385, 1.000000000000000000, 0.9238795325112867385, 1.000000000000000000, 0.9238795325112867385, 1.000000000000000000, 0.9754817479996107377, 0.9667580569362973497 ) ) 
 REPRESENTATION_ITEM ( '' )  );
#16846 = DIRECTION ( 'NONE',  ( -0.000000000000000000, 0.000000000000000000, -1.000000000000000000 ) ) ;
#16847 = CARTESIAN_POINT ( 'NONE',  ( 1.960495238260606010, -8.383787449798761671, 1.627490053312942164 ) ) ;
#16848 = CARTESIAN_POINT ( 'NONE',  ( 13.42791111847407848, 4.999999999999999112, 0.000000000000000000 ) ) ;
#16849 = CARTESIAN_POINT ( 'NONE',  ( -12.66835678905406049, -17.31048215276408797, 4.799178440007564994 ) ) ;
#16850 = CARTESIAN_POINT ( 'NONE',  ( 10.74655858231679417, -21.94931252712234482, 5.250000000000000888 ) ) ;
#16851 = CARTESIAN_POINT ( 'NONE',  ( -13.77324158252158171, -0.8888000826463379189, 6.637859435864801760 ) ) ;
#16852 = EDGE_CURVE ( 'NONE', #6003, #7246, #4189, .T. ) ;
#16853 = DIRECTION ( 'NONE',  ( 1.000000000000000000, 5.204170427930411817E-15, -0.000000000000000000 ) ) ;
#16854 = CARTESIAN_POINT ( 'NONE',  ( 10.74655858231679417, -21.94931252712234482, 5.250000000000000888 ) ) ;
#16855 = CARTESIAN_POINT ( 'NONE',  ( 5.784691417683179182, -23.77099543870834353, 4.174186261275252718 ) ) ;
#16856 = CARTESIAN_POINT ( 'NONE',  ( -9.527808582316792396, -23.72900456129165647, 4.275561207030568411 ) ) ;
#16857 = ORIENTED_EDGE ( 'NONE', *, *, #12184, .F. ) ;
#16858 = CARTESIAN_POINT ( 'NONE',  ( 12.66503773474750894, -18.97809439524806052, 6.263381662489337920 ) ) ;
#16859 = CARTESIAN_POINT ( 'NONE',  ( 13.08739618700683849, 3.851007443844064237, 5.254256565007597857 ) ) ;
#16860 = CARTESIAN_POINT ( 'NONE',  ( 15.00000000000001421, -25.49999999999999645, 4.000000000000000000 ) ) ;
#16861 = VERTEX_POINT ( 'NONE', #7594 ) ;
#16862 = VERTEX_POINT ( 'NONE', #4460 ) ;
#16863 = DIRECTION ( 'NONE',  ( 0.000000000000000000, -0.000000000000000000, 1.000000000000000000 ) ) ;
#16864 = CARTESIAN_POINT ( 'NONE',  ( -12.64691428603184242, -19.14332855539073464, 5.509795676248469221 ) ) ;
#16865 = DIRECTION ( 'NONE',  ( -0.000000000000000000, -0.000000000000000000, -1.000000000000000000 ) ) ;
#16866 = CARTESIAN_POINT ( 'NONE',  ( -13.39662663169496781, -19.15785509940297615, 5.494950532956567102 ) ) ;
#16867 = DIRECTION ( 'NONE',  ( -1.000000000000000000, -2.312964634635730039E-15, 0.000000000000000000 ) ) ;
#16868 = CARTESIAN_POINT ( 'NONE',  ( 2.731427961995660958, -10.89409100229510052, 2.829571171190552015 ) ) ;
#16869 = PLANE ( 'NONE',  #3474 ) ;
#16870 = DIRECTION ( 'NONE',  ( 0.000000000000000000, -1.000000000000000000, 0.000000000000000000 ) ) ;
#16871 = VECTOR ( 'NONE', #14371, 1000.000000000000000 ) ;
#16872 = DIRECTION ( 'NONE',  ( -0.000000000000000000, -0.000000000000000000, -1.000000000000000000 ) ) ;
#16873 = CARTESIAN_POINT ( 'NONE',  ( -9.527808582316795949, -24.47900456129166358, 4.586221378810390270 ) ) ;
#16874 = CARTESIAN_POINT ( 'NONE',  ( -1.960495238260606010, -8.383787449798761671, 1.627490053312942164 ) ) ;
#16875 = ORIENTED_EDGE ( 'NONE', *, *, #17638, .T. ) ;
#16876 = CARTESIAN_POINT ( 'NONE',  ( -13.81612658856640863, 2.776892722604777930, 5.216624963382545666 ) ) ;
#16877 = CARTESIAN_POINT ( 'NONE',  ( -5.999999999999999112, -2.500000000000047518, 9.999999999999998224 ) ) ;
#16878 = ADVANCED_FACE ( 'NONE', ( #2678 ), #8857, .T. ) ;
#16879 = CARTESIAN_POINT ( 'NONE',  ( 4.934058582316795061, -23.73192549717337130, 5.303608408759367343 ) ) ;
#16880 = CARTESIAN_POINT ( 'NONE',  ( -9.534691417683177406, -20.97900456129164581, 3.136473910504570917 ) ) ;
#16881 = ORIENTED_EDGE ( 'NONE', *, *, #14969, .F. ) ;
#16882 = CARTESIAN_POINT ( 'NONE',  ( 13.37499999999998224, -20.24999999999991829, 4.333333333333343695 ) ) ;
#16883 = DIRECTION ( 'NONE',  ( -0.000000000000000000, -0.000000000000000000, -1.000000000000000000 ) ) ;
#16884 = VERTEX_POINT ( 'NONE', #12291 ) ;
#16885 = AXIS2_PLACEMENT_3D ( 'NONE', #3532, #14820, #17762 ) ;
#16886 = ORIENTED_EDGE ( 'NONE', *, *, #17706, .F. ) ;
#16887 = CARTESIAN_POINT ( 'NONE',  ( -20.49999999999998224, -21.99999999999999645, 11.00000000000000178 ) ) ;
#16888 = VERTEX_POINT ( 'NONE', #15535 ) ;
#16889 = CARTESIAN_POINT ( 'NONE',  ( -13.58606361274418184, -9.591287556442823714, 5.700679699621803209 ) ) ;
#16890 = ADVANCED_FACE ( 'NONE', ( #9164 ), #20260, .F. ) ;
#16891 = ORIENTED_EDGE ( 'NONE', *, *, #594, .T. ) ;
#16892 = CARTESIAN_POINT ( 'NONE',  ( 0.000000000000000000, 11.64110105645932691, 10.00000000000000000 ) ) ;
#16893 = CARTESIAN_POINT ( 'NONE',  ( 0.000000000000000000, 11.64110105645932691, 10.00000000000000000 ) ) ;
#16894 = CARTESIAN_POINT ( 'NONE',  ( 0.000000000000000000, 9.000000000000001776, 1.000000000000000000 ) ) ;
#16895 = CARTESIAN_POINT ( 'NONE',  ( 1.513434189748285918, -8.364917468222230923, 2.372643865078341019 ) ) ;
#16896 = LINE ( 'NONE', #2466, #3192 ) ;
#16897 = CARTESIAN_POINT ( 'NONE',  ( 13.89075858682503650, 5.045808634669852744, 6.406973581600956535 ) ) ;
#16898 = DIRECTION ( 'NONE',  ( 0.000000000000000000, 1.000000000000000000, -0.000000000000000000 ) ) ;
#16899 = DIRECTION ( 'NONE',  ( 1.000000000000000000, 0.000000000000000000, 0.000000000000000000 ) ) ;
#16900 = CARTESIAN_POINT ( 'NONE',  ( -13.17791111847408025, 0.000000000000000000, 1.000000000000000000 ) ) ;
#16901 = CARTESIAN_POINT ( 'NONE',  ( 10.37844141768317741, -22.99999999999999645, 3.449312527122335048 ) ) ;
#16902 = CARTESIAN_POINT ( 'NONE',  ( -12.63819864697926754, -19.58346832754827105, 5.450273968536036406 ) ) ;
#16903 = CARTESIAN_POINT ( 'NONE',  ( -6.440941417683175629, -21.25705176302044208, 2.828734674606458555 ) ) ;
#16904 = EDGE_CURVE ( 'NONE', #19089, #6994, #8952, .T. ) ;
#16905 = CARTESIAN_POINT ( 'NONE',  ( -9.722191417683177406, -19.52099543870834353, 4.586221378810406257 ) ) ;
#16906 = ORIENTED_EDGE ( 'NONE', *, *, #14634, .T. ) ;
#16907 = CARTESIAN_POINT ( 'NONE',  ( 12.63298722613685676, -19.09664508008815531, 4.760766981674283471 ) ) ;
#16908 = CARTESIAN_POINT ( 'NONE',  ( -12.65051119073526564, -18.96168486786632457, 5.513701926248478102 ) ) ;
#16909 = VERTEX_POINT ( 'NONE', #12091 ) ;
#16910 = PLANE ( 'NONE',  #17287 ) ;
#16911 = CARTESIAN_POINT ( 'NONE',  ( 14.31494360078803041, 10.00000000000000000, 1.000000000000000000 ) ) ;
#16912 = ORIENTED_EDGE ( 'NONE', *, *, #14969, .T. ) ;
#16913 = CARTESIAN_POINT ( 'NONE',  ( 1.872293763630120678, -10.04602735435188698, 2.419156501869924369 ) ) ;
#16914 = VECTOR ( 'NONE', #8209, 1000.000000000000000 ) ;
#16915 = EDGE_LOOP ( 'NONE', ( #5867, #11364, #18667, #811 ) ) ;
#16916 = ORIENTED_EDGE ( 'NONE', *, *, #1860, .T. ) ;
#16917 = DIRECTION ( 'NONE',  ( 1.000000000000000000, 0.000000000000000000, 0.000000000000000000 ) ) ;
#16918 = DIRECTION ( 'NONE',  ( 1.000000000000000000, 0.000000000000000000, 0.000000000000000000 ) ) ;
#16919 = CARTESIAN_POINT ( 'NONE',  ( -1.733187991654075777, -9.867296153774269385, 1.623254759047128237 ) ) ;
#16920 = CARTESIAN_POINT ( 'NONE',  ( 13.49999999999998401, -18.49999999999999645, 4.000000000000000000 ) ) ;
#16921 = CARTESIAN_POINT ( 'NONE',  ( 0.000000000000000000, 0.000000000000000000, 1.000000000000000000 ) ) ;
#16922 = CARTESIAN_POINT ( 'NONE',  ( -22.81633994409548549, 10.00000000000000000, 0.000000000000000000 ) ) ;
#16923 = CARTESIAN_POINT ( 'NONE',  ( 11.97219141768317918, -24.47900456129165292, 2.413778621189595963 ) ) ;
#16924 = CARTESIAN_POINT ( 'NONE',  ( -12.63249216759192350, -19.87164553660301536, 5.297612231341934041 ) ) ;
#16925 = CARTESIAN_POINT ( 'NONE',  ( -8.878441417683177406, -24.50000000000000000, 3.449312527122335048 ) ) ;
#16926 = EDGE_CURVE ( 'NONE', #5036, #11811, #15436, .T. ) ;
#16927 = ORIENTED_EDGE ( 'NONE', *, *, #20290, .T. ) ;
#16928 = EDGE_CURVE ( 'NONE', #19095, #49, #1005, .T. ) ;
#16929 = CARTESIAN_POINT ( 'NONE',  ( 11.77780858231679417, -20.27099543870833642, 2.724438792969431589 ) ) ;
#16930 = CARTESIAN_POINT ( 'NONE',  ( 21.67243175760212637, 4.999999999999999112, 0.000000000000000000 ) ) ;
#16931 = CARTESIAN_POINT ( 'NONE',  ( -13.87372783958217681, 4.185755898898970706, 6.732634959205082481 ) ) ;
#16932 = CARTESIAN_POINT ( 'NONE',  ( 6.246558582316795949, -21.94931252712234127, 4.499999999999999112 ) ) ;
#16933 = DIRECTION ( 'NONE',  ( 0.000000000000000000, -0.000000000000000000, 1.000000000000000000 ) ) ;
#16934 = ORIENTED_EDGE ( 'NONE', *, *, #8787, .T. ) ;
#16935 = ORIENTED_EDGE ( 'NONE', *, *, #20543, .F. ) ;
#16936 = CARTESIAN_POINT ( 'NONE',  ( 13.40787921250184311, -19.33959976865745389, 6.241060671539915283 ) ) ;
#16937 = CARTESIAN_POINT ( 'NONE',  ( 15.00000000000001776, -26.49999999999999645, 4.000000000000000000 ) ) ;
#16938 = ORIENTED_EDGE ( 'NONE', *, *, #15013, .T. ) ;
#16939 = LINE ( 'NONE', #5656, #10810 ) ;
#16940 = ORIENTED_EDGE ( 'NONE', *, *, #690, .F. ) ;
#16941 = CARTESIAN_POINT ( 'NONE',  ( -12.43405858231679417, -23.20159541128345992, 4.773278322869455970 ) ) ;
#16942 = CARTESIAN_POINT ( 'NONE',  ( -5.563547257480587760, 0.000000000000000000, 1.000000000000000000 ) ) ;
#16943 = DIRECTION ( 'NONE',  ( 0.000000000000000000, -0.000000000000000000, 1.000000000000000000 ) ) ;
#16944 = CARTESIAN_POINT ( 'NONE',  ( 2.762374231067749708, -9.968169115173667549, 1.841775933429679268 ) ) ;
#16945 = LINE ( 'NONE', #17161, #9727 ) ;
#16946 = CARTESIAN_POINT ( 'NONE',  ( -13.37500003877585186, -19.49999804181952712, 4.520055687292853008 ) ) ;
#16947 = CARTESIAN_POINT ( 'NONE',  ( 11.77780858231679417, -20.27099543870833642, 2.724438792969431589 ) ) ;
#16948 = CARTESIAN_POINT ( 'NONE',  ( -13.40995420747273670, -19.23481252262645924, 6.243328185864100988 ) ) ;
#16949 = ADVANCED_FACE ( 'NONE', ( #18794 ), #18483, .T. ) ;
#16950 = ADVANCED_FACE ( 'NONE', ( #17208 ), #14067, .T. ) ;
#16951 = DIRECTION ( 'NONE',  ( 1.000000000000000000, 0.000000000000000000, 0.000000000000000000 ) ) ;
#16952 = CARTESIAN_POINT ( 'NONE',  ( 6.246558582316795949, -21.94931252712234127, 4.499999999999999112 ) ) ;
#16953 = CARTESIAN_POINT ( 'NONE',  ( 5.222191417683178294, -20.27099543870833998, 4.275561207030583510 ) ) ;
#16954 = CARTESIAN_POINT ( 'NONE',  ( -12.80905858231679417, -23.27327832286945153, 2.298404588716537411 ) ) ;
#16955 = ORIENTED_EDGE ( 'NONE', *, *, #492, .F. ) ;
#16956 = CARTESIAN_POINT ( 'NONE',  ( 13.09560264576187905, 4.265433610975056133, 4.333333333333380999 ) ) ;
#16957 = DIRECTION ( 'NONE',  ( -1.000000000000000000, 0.000000000000000000, 0.000000000000000000 ) ) ;
#16958 = ORIENTED_EDGE ( 'NONE', *, *, #3849, .T. ) ;
#16959 = VECTOR ( 'NONE', #10020, 1000.000000000000000 ) ;
#16960 = UNCERTAINTY_MEASURE_WITH_UNIT (LENGTH_MEASURE( 1.000000000000000082E-05 ), #14952, 'distance_accuracy_value', 'NONE');
#16961 =( BOUNDED_SURFACE ( )  B_SPLINE_SURFACE ( 3, 3, ( 
 ( #6022, #10936, #17415, #15839, #12395, #14259, #2882, #6326, #9564, #12498, #2987, #5145, #9259, #15937, #4757, #18894, #4553, #9364, #1617, #15738, #14164, #12699, #19102, #751, #5242, #7233, #539, #19900, #6916, #15175, #11928, #13190, #19586, #5664, #12035, #18429, #19801, #18322, #11619, #5350 ),
 ( #14765, #16435, #441, #6821, #13397, #15070, #19999, #2308, #18007, #5557, #8807, #10369, #3677, #19687, #10164, #14960, #5457, #9950, #10064, #13287, #2111, #3986, #3882, #16629, #16333, #11828, #8494, #14863, #16745, #8698, #11728, #16533, #18121, #2416, #2008, #3784, #7137, #2209, #8591, #641 ),
 ( #7029, #18219, #8395, #10262, #13501, #851, #13597, #17253, #15483, #4093, #2934, #6178, #18739, #7643, #18633, #15381, #17160, #15271, #4296, #9313, #4507, #18532, #1165, #5871, #1372, #16847, #8906, #12240, #10478, #6082, #10891, #7753, #15689, #20108, #14118, #20211, #20421, #13701, #20525, #14013 ),
 ( #10681, #2514, #5971, #17055, #951, #12546, #13807, #7339, #5770, #10577, #12142, #4195, #7545, #9211, #16944, #2836, #2618, #12451, #9010, #1066, #7445, #2734, #9114, #13908, #20308, #12345, #4407, #10791, #15583, #18845, #1267, #8061, #18943, #17567, #4706, #6272, #3346, #108, #15792, #20719 ),
 ( #14425, #14531, #14212, #15890, #12645, #6494, #6388, #1778, #1568, #19051, #19359, #4598, #12755, #12855, #19257, #8165, #11192, #10990, #206, #17360, #4909, #9724, #19159, #7944, #11288, #7850, #4813, #12956, #6590, #11097, #9613, #3241, #5015, #1470, #20621, #15996, #3045, #9422, #17468, #3145 ),
 ( #9516, #14314, #1674, #17672, #16109, #7609, #10861, #10754, #17125, #15343, #18811, #2805, #16913, #9385, #5937, #13776, #12417, #20180, #13978, #18914, #1136, #12308, #15759, #7415, #4572, #6148, #10645, #12208, #1442, #12517, #9179, #7820, #17018, #15554, #7716, #18599, #14182, #7514, #10957, #13877 ),
 ( #19018, #20493, #1340, #20278, #4672, #2696, #3008, #14086, #4370, #5840, #17325, #20382, #6047, #20590, #6242, #18705, #12614, #2586, #4478, #8970, #17225, #1026, #4262, #9083, #1234, #15452, #2903, #9279, #15653, #11315, #6614, #17487, #13262, #14232, #20640, #7002, #13369, #19772, #133, #19659 ) ),
 .UNSPECIFIED., .T., .F., .T. ) 
 B_SPLINE_SURFACE_WITH_KNOTS ( ( 4, 3, 4 ),
 ( 4, 2, 2, 2, 2, 2, 2, 2, 2, 2, 2, 2, 2, 2, 2, 2, 2, 2, 2, 4 ),
 ( 0.000000000000000000, 0.5000000000000000000, 1.000000000000000000 ),
 ( 0.000000000000000000, 0.3100443560520446118, 0.4650665340780669177, 0.5425776230910780429, 0.5813331675975836887, 0.6007109398508364562, 0.6200887121040892236, 0.6309950902025724950, 0.6419014683010558775, 0.6637142244980225314, 0.7073397368919559502, 0.7509652492858893691, 0.7727780054828560230, 0.7836843835813394055, 0.7945907616798226769, 0.8074288390748337596, 0.8202669164698448423, 0.8459430712598670077, 0.8972953808399113385, 1.000000000000000000 ),
 .UNSPECIFIED. ) 
 GEOMETRIC_REPRESENTATION_ITEM ( )  RATIONAL_B_SPLINE_SURFACE ( (
 ( 1.000000000000000000, 1.000000000000000000, 1.000000000000000000, 1.000000000000000000, 1.000000000000000000, 1.000000000000000000, 1.000000000000000000, 1.000000000000000000, 1.000000000000000000, 1.000000000000000000, 1.000000000000000000, 1.000000000000000000, 1.000000000000000000, 1.000000000000000000, 1.000000000000000000, 1.000000000000000000, 1.000000000000000000, 1.000000000000000000, 1.000000000000000000, 1.000000000000000000, 1.000000000000000000, 1.000000000000000000, 1.000000000000000000, 1.000000000000000000, 1.000000000000000000, 1.000000000000000000, 1.000000000000000000, 1.000000000000000000, 1.000000000000000000, 1.000000000000000000, 1.000000000000000000, 1.000000000000000000, 1.000000000000000000, 1.000000000000000000, 1.000000000000000000, 1.000000000000000000, 1.000000000000000000, 1.000000000000000000, 1.000000000000000000, 1.000000000000000000),
 ( 0.3333333333333333703, 0.3333333333333333703, 0.3333333333333333703, 0.3333333333333333703, 0.3333333333333333703, 0.3333333333333333703, 0.3333333333333333703, 0.3333333333333333703, 0.3333333333333333703, 0.3333333333333333703, 0.3333333333333333703, 0.3333333333333333703, 0.3333333333333333703, 0.3333333333333333703, 0.3333333333333333703, 0.3333333333333333703, 0.3333333333333333703, 0.3333333333333333703, 0.3333333333333333703, 0.3333333333333333703, 0.3333333333333333703, 0.3333333333333333703, 0.3333333333333333703, 0.3333333333333333703, 0.3333333333333333703, 0.3333333333333333703, 0.3333333333333333703, 0.3333333333333333703, 0.3333333333333333703, 0.3333333333333333703, 0.3333333333333333703, 0.3333333333333333703, 0.3333333333333333703, 0.3333333333333333703, 0.3333333333333333703, 0.3333333333333333703, 0.3333333333333333703, 0.3333333333333333703, 0.3333333333333333703, 0.3333333333333333703),
 ( 0.3333333333333333703, 0.3333333333333333703, 0.3333333333333333703, 0.3333333333333333703, 0.3333333333333333703, 0.3333333333333333703, 0.3333333333333333703, 0.3333333333333333703, 0.3333333333333333703, 0.3333333333333333703, 0.3333333333333333703, 0.3333333333333333703, 0.3333333333333333703, 0.3333333333333333703, 0.3333333333333333703, 0.3333333333333333703, 0.3333333333333333703, 0.3333333333333333703, 0.3333333333333333703, 0.3333333333333333703, 0.3333333333333333703, 0.3333333333333333703, 0.3333333333333333703, 0.3333333333333333703, 0.3333333333333333703, 0.3333333333333333703, 0.3333333333333333703, 0.3333333333333333703, 0.3333333333333333703, 0.3333333333333333703, 0.3333333333333333703, 0.3333333333333333703, 0.3333333333333333703, 0.3333333333333333703, 0.3333333333333333703, 0.3333333333333333703, 0.3333333333333333703, 0.3333333333333333703, 0.3333333333333333703, 0.3333333333333333703),
 ( 1.000000000000000000, 1.000000000000000000, 1.000000000000000000, 1.000000000000000000, 1.000000000000000000, 1.000000000000000000, 1.000000000000000000, 1.000000000000000000, 1.000000000000000000, 1.000000000000000000, 1.000000000000000000, 1.000000000000000000, 1.000000000000000000, 1.000000000000000000, 1.000000000000000000, 1.000000000000000000, 1.000000000000000000, 1.000000000000000000, 1.000000000000000000, 1.000000000000000000, 1.000000000000000000, 1.000000000000000000, 1.000000000000000000, 1.000000000000000000, 1.000000000000000000, 1.000000000000000000, 1.000000000000000000, 1.000000000000000000, 1.000000000000000000, 1.000000000000000000, 1.000000000000000000, 1.000000000000000000, 1.000000000000000000, 1.000000000000000000, 1.000000000000000000, 1.000000000000000000, 1.000000000000000000, 1.000000000000000000, 1.000000000000000000, 1.000000000000000000),
 ( 0.3333333333333333703, 0.3333333333333333703, 0.3333333333333333703, 0.3333333333333333703, 0.3333333333333333703, 0.3333333333333333703, 0.3333333333333333703, 0.3333333333333333703, 0.3333333333333333703, 0.3333333333333333703, 0.3333333333333333703, 0.3333333333333333703, 0.3333333333333333703, 0.3333333333333333703, 0.3333333333333333703, 0.3333333333333333703, 0.3333333333333333703, 0.3333333333333333703, 0.3333333333333333703, 0.3333333333333333703, 0.3333333333333333703, 0.3333333333333333703, 0.3333333333333333703, 0.3333333333333333703, 0.3333333333333333703, 0.3333333333333333703, 0.3333333333333333703, 0.3333333333333333703, 0.3333333333333333703, 0.3333333333333333703, 0.3333333333333333703, 0.3333333333333333703, 0.3333333333333333703, 0.3333333333333333703, 0.3333333333333333703, 0.3333333333333333703, 0.3333333333333333703, 0.3333333333333333703, 0.3333333333333333703, 0.3333333333333333703),
 ( 0.3333333333333333703, 0.3333333333333333703, 0.3333333333333333703, 0.3333333333333333703, 0.3333333333333333703, 0.3333333333333333703, 0.3333333333333333703, 0.3333333333333333703, 0.3333333333333333703, 0.3333333333333333703, 0.3333333333333333703, 0.3333333333333333703, 0.3333333333333333703, 0.3333333333333333703, 0.3333333333333333703, 0.3333333333333333703, 0.3333333333333333703, 0.3333333333333333703, 0.3333333333333333703, 0.3333333333333333703, 0.3333333333333333703, 0.3333333333333333703, 0.3333333333333333703, 0.3333333333333333703, 0.3333333333333333703, 0.3333333333333333703, 0.3333333333333333703, 0.3333333333333333703, 0.3333333333333333703, 0.3333333333333333703, 0.3333333333333333703, 0.3333333333333333703, 0.3333333333333333703, 0.3333333333333333703, 0.3333333333333333703, 0.3333333333333333703, 0.3333333333333333703, 0.3333333333333333703, 0.3333333333333333703, 0.3333333333333333703),
 ( 1.000000000000000000, 1.000000000000000000, 1.000000000000000000, 1.000000000000000000, 1.000000000000000000, 1.000000000000000000, 1.000000000000000000, 1.000000000000000000, 1.000000000000000000, 1.000000000000000000, 1.000000000000000000, 1.000000000000000000, 1.000000000000000000, 1.000000000000000000, 1.000000000000000000, 1.000000000000000000, 1.000000000000000000, 1.000000000000000000, 1.000000000000000000, 1.000000000000000000, 1.000000000000000000, 1.000000000000000000, 1.000000000000000000, 1.000000000000000000, 1.000000000000000000, 1.000000000000000000, 1.000000000000000000, 1.000000000000000000, 1.000000000000000000, 1.000000000000000000, 1.000000000000000000, 1.000000000000000000, 1.000000000000000000, 1.000000000000000000, 1.000000000000000000, 1.000000000000000000, 1.000000000000000000, 1.000000000000000000, 1.000000000000000000, 1.000000000000000000) ) ) 
 REPRESENTATION_ITEM ( '' )  SURFACE ( )  );
#16962 = ORIENTED_EDGE ( 'NONE', *, *, #7798, .F. ) ;
#16963 = DIRECTION ( 'NONE',  ( 0.000000000000000000, 1.000000000000000000, 0.000000000000000000 ) ) ;
#16964 = ADVANCED_FACE ( 'NONE', ( #12501 ), #10625, .F. ) ;
#16965 = CARTESIAN_POINT ( 'NONE',  ( -12.64571531779736979, -19.20387645123237164, 5.508493592915143289 ) ) ;
#16966 = CARTESIAN_POINT ( 'NONE',  ( -2.623717082130370137, -10.12934627674766830, 2.633169448359191644 ) ) ;
#16967 = CARTESIAN_POINT ( 'NONE',  ( -13.38921792038197900, -19.53199502070850357, 5.456033026503027017 ) ) ;
#16968 = COLOUR_RGB ( '', 0.72549020, 0.75294118, 0.79215686) ;
#16969 = CARTESIAN_POINT ( 'NONE',  ( 0.000000000000000000, -9.114917468222230923, 1.997643865078340797 ) ) ;
#16970 = DIRECTION ( 'NONE',  ( 1.000000000000000000, 0.000000000000000000, 0.000000000000000000 ) ) ;
#16971 = PLANE ( 'NONE',  #7489 ) ;
#16972 = VECTOR ( 'NONE', #17233, 1000.000000000000000 ) ;
#16973 = CYLINDRICAL_SURFACE ( 'NONE', #14406, 1.499999999999999556 ) ;
#16974 = LINE ( 'NONE', #2650, #13309 ) ;
#16975 = CARTESIAN_POINT ( 'NONE',  ( -12.24655858231679595, -21.94931252712234127, 6.000000000000001776 ) ) ;
#16976 = CARTESIAN_POINT ( 'NONE',  ( -1.731569788986178304, -8.364930642962441709, 1.622647248614820015 ) ) ;
#16977 = EDGE_LOOP ( 'NONE', ( #19604, #9510, #943, #11339 ) ) ;
#16978 = CARTESIAN_POINT ( 'NONE',  ( -13.84256985046264710, 4.112277448363203192, 5.213861325540929847 ) ) ;
#16979 = DIRECTION ( 'NONE',  ( -1.040834085586084454E-15, 1.000000000000000000, 8.673617379884037444E-16 ) ) ;
#16980 = CARTESIAN_POINT ( 'NONE',  ( 9.628441417683177406, -19.49999999999998934, 3.550687472877664952 ) ) ;
#16981 = CARTESIAN_POINT ( 'NONE',  ( -12.62844141768317741, -20.99999999999999645, 3.550687472877664952 ) ) ;
#16982 = ORIENTED_EDGE ( 'NONE', *, *, #18688, .F. ) ;
#16983 = CARTESIAN_POINT ( 'NONE',  ( 13.83065313257865370, 2.760483195222930952, 5.966304699623404595 ) ) ;
#16984 = CARTESIAN_POINT ( 'NONE',  ( 15.00000000000001776, -26.49999999999999645, 4.000000000000000000 ) ) ;
#16985 = CIRCLE ( 'NONE', #3967, 2.999999999999999112 ) ;
#16986 = ORIENTED_EDGE ( 'NONE', *, *, #19336, .T. ) ;
#16987 = ORIENTED_EDGE ( 'NONE', *, *, #3709, .T. ) ;
#16988 = FACE_BOUND ( 'NONE', #14029, .T. ) ;
#16989 = AXIS2_PLACEMENT_3D ( 'NONE', #17084, #12068, #4220 ) ;
#16990 = ORIENTED_EDGE ( 'NONE', *, *, #9361, .F. ) ;
#16991 = CARTESIAN_POINT ( 'NONE',  ( -13.47096266223369376, -15.40388555723029462, 5.575679699623145247 ) ) ;
#16992 = AXIS2_PLACEMENT_3D ( 'NONE', #2589, #12214, #918 ) ;
#16993 = CARTESIAN_POINT ( 'NONE',  ( 1.407845757905374695, -9.114917468222230923, 2.372643865078341019 ) ) ;
#16994 = VERTEX_POINT ( 'NONE', #16797 ) ;
#16995 = DIRECTION ( 'NONE',  ( -0.000000000000000000, -0.000000000000000000, -1.000000000000000000 ) ) ;
#16996 = LINE ( 'NONE', #694, #11343 ) ;
#16997 = EDGE_CURVE ( 'NONE', #17851, #18752, #16896, .T. ) ;
#16998 = AXIS2_PLACEMENT_3D ( 'NONE', #15966, #11073, #10867 ) ;
#16999 = LINE ( 'NONE', #7283, #4316 ) ;
#17000 = VECTOR ( 'NONE', #13644, 1000.000000000000000 ) ;
#17001 = CARTESIAN_POINT ( 'NONE',  ( 0.5631383031621635116, -9.114917468222230923, 2.372643865078341019 ) ) ;
#17002 = DIRECTION ( 'NONE',  ( -1.000000000000000000, 0.000000000000000000, -0.000000000000000000 ) ) ;
#17003 = VECTOR ( 'NONE', #12535, 1000.000000000000000 ) ;
#17004 = DIRECTION ( 'NONE',  ( 1.000000000000000000, 0.000000000000000000, 0.000000000000000000 ) ) ;
#17005 = LINE ( 'NONE', #5725, #15383 ) ;
#17006 = CARTESIAN_POINT ( 'NONE',  ( 8.119520639128047890, 4.999999999999999112, 1.000000000000000000 ) ) ;
#17007 = CARTESIAN_POINT ( 'NONE',  ( 5.128441417683177406, -20.24999999999999289, 3.550687472877664952 ) ) ;
#17008 = CARTESIAN_POINT ( 'NONE',  ( -12.62500016093973620, -20.24999187254239175, 4.532396751752561848 ) ) ;
#17009 = CARTESIAN_POINT ( 'NONE',  ( -12.62155858231679417, -22.99999999999999645, 3.550687472877652073 ) ) ;
#17010 = CARTESIAN_POINT ( 'NONE',  ( -8.128441417683177406, -19.49999999999998934, 3.550687472877664952 ) ) ;
#17011 = ORIENTED_EDGE ( 'NONE', *, *, #5509, .F. ) ;
#17012 = CARTESIAN_POINT ( 'NONE',  ( 13.12529397354238192, 5.014845663890295846, 4.166666666666765551 ) ) ;
#17013 = CARTESIAN_POINT ( 'NONE',  ( -13.12529397353891270, 5.014845663890295846, 3.333333333333220239 ) ) ;
#17014 = ORIENTED_EDGE ( 'NONE', *, *, #10117, .T. ) ;
#17015 = CARTESIAN_POINT ( 'NONE',  ( -6.313547257480587760, 10.00000000000000000, 1.000000000000000000 ) ) ;
#17016 = CARTESIAN_POINT ( 'NONE',  ( 19.23630159782011617, 0.000000000000000000, 1.000000000000000000 ) ) ;
#17017 = VERTEX_POINT ( 'NONE', #7397 ) ;
#17018 = CARTESIAN_POINT ( 'NONE',  ( 1.513434189748285918, -9.864917468222230923, 2.372643865078341019 ) ) ;
#17019 = VECTOR ( 'NONE', #7249, 1000.000000000000000 ) ;
#17020 = ORIENTED_EDGE ( 'NONE', *, *, #14205, .T. ) ;
#17021 = CARTESIAN_POINT ( 'NONE',  ( 10.18924542913430820, 16.00000000000000000, 1.000000000000000000 ) ) ;
#17022 = DIRECTION ( 'NONE',  ( -0.000000000000000000, -0.000000000000000000, -1.000000000000000000 ) ) ;
#17023 = AXIS2_PLACEMENT_3D ( 'NONE', #12757, #20526, #9314 ) ;
#17024 = EDGE_CURVE ( 'NONE', #17249, #2461, #13647, .T. ) ;
#17025 = CARTESIAN_POINT ( 'NONE',  ( -1.776440835594205847, -9.874406767442327038, 1.625080906685880233 ) ) ;
#17026 = DIRECTION ( 'NONE',  ( 0.000000000000000000, 1.000000000000000000, -0.000000000000000000 ) ) ;
#17027 = DIRECTION ( 'NONE',  ( 0.000000000000000000, 1.000000000000000000, -0.000000000000000000 ) ) ;
#17028 = CARTESIAN_POINT ( 'NONE',  ( 14.50000000000001243, -18.49999999999999645, 1.000000000000000000 ) ) ;
#17029 = ADVANCED_FACE ( 'NONE', ( #20160 ), #17307, .T. ) ;
#17030 = EDGE_CURVE ( 'NONE', #5395, #20292, #58, .T. ) ;
#17031 = CARTESIAN_POINT ( 'NONE',  ( 12.15969141768317918, -22.98484643305507191, 0.9790045612916508100 ) ) ;
#17032 = CARTESIAN_POINT ( 'NONE',  ( -13.00900269284621302, -0.8578640112522492034, 5.903024842915844062 ) ) ;
#17033 = CARTESIAN_POINT ( 'NONE',  ( -9.065941417683177406, -23.20159541128344927, 2.226721677130534705 ) ) ;
#17034 = STYLED_ITEM ( 'NONE', ( #16326 ), #4314 ) ;
#17035 = EDGE_LOOP ( 'NONE', ( #8797, #19818, #9581, #1353 ) ) ;
#17036 = PLANE ( 'NONE',  #9615 ) ;
#17037 = CARTESIAN_POINT ( 'NONE',  ( -3.500698171653725765, 10.00000000000000000, 1.000000000000000000 ) ) ;
#17038 = CARTESIAN_POINT ( 'NONE',  ( -13.37499999999998224, -20.99999999999998934, 4.166666666666637653 ) ) ;
#17039 = VECTOR ( 'NONE', #16660, 1000.000000000000000 ) ;
#17040 = CARTESIAN_POINT ( 'NONE',  ( 9.902808582316794173, -22.77556120703056308, 1.770995438708339975 ) ) ;
#17041 = DIRECTION ( 'NONE',  ( -3.469446951953611033E-15, 1.000000000000000000, 0.000000000000000000 ) ) ;
#17042 = VERTEX_POINT ( 'NONE', #6443 ) ;
#17043 = VERTEX_POINT ( 'NONE', #11240 ) ;
#17044 = CARTESIAN_POINT ( 'NONE',  ( 13.84517967659089521, 2.744073667841084418, 6.715984435864265301 ) ) ;
#17045 = DIRECTION ( 'NONE',  ( 0.000000000000000000, -0.000000000000000000, 1.000000000000000000 ) ) ;
#17046 =( LENGTH_UNIT ( ) NAMED_UNIT ( * ) SI_UNIT ( .MILLI., .METRE. ) );
#17047 = ORIENTED_EDGE ( 'NONE', *, *, #9956, .T. ) ;
#17048 = CARTESIAN_POINT ( 'NONE',  ( -11.75209451496117197, 0.000000000000000000, 1.000000000000000000 ) ) ;
#17049 = ORIENTED_EDGE ( 'NONE', *, *, #17412, .F. ) ;
#17050 = CARTESIAN_POINT ( 'NONE',  ( -8.309058582316792396, -23.27327832286945153, 2.298404588716537411 ) ) ;
#17051 = PLANE ( 'NONE',  #8600 ) ;
#17052 = EDGE_CURVE ( 'NONE', #5289, #4330, #14480, .T. ) ;
#17053 = VECTOR ( 'NONE', #4305, 1000.000000000000114 ) ;
#17054 = CARTESIAN_POINT ( 'NONE',  ( 15.86404127825609400, 4.999999999999999112, 1.000000000000000000 ) ) ;
#17055 = CARTESIAN_POINT ( 'NONE',  ( 3.059891148793807414, -12.07002330923453570, 2.381574079220715401 ) ) ;
#17056 = VECTOR ( 'NONE', #2656, 1000.000000000000000 ) ;
#17057 = CARTESIAN_POINT ( 'NONE',  ( -4.250698171653726654, 0.000000000000000000, 1.000000000000000000 ) ) ;
#17058 = CARTESIAN_POINT ( 'NONE',  ( -13.09073190589589331, 4.019461247742575516, 5.257453802652931607 ) ) ;
#17059 = CARTESIAN_POINT ( 'NONE',  ( 12.71530858231679240, -23.77099543870833998, 2.825813738724734847 ) ) ;
#17060 = CARTESIAN_POINT ( 'NONE',  ( -13.37499999999998224, -21.00000000000006395, 4.416666666666682062 ) ) ;
#17061 = DIRECTION ( 'NONE',  ( -0.000000000000000000, -0.000000000000000000, -1.000000000000000000 ) ) ;
#17062 = CARTESIAN_POINT ( 'NONE',  ( 9.809058582316794173, -23.27327832286945153, 2.298404588716537411 ) ) ;
#17063 = CARTESIAN_POINT ( 'NONE',  ( 4.378441417683176518, -23.74999999999999645, 3.449312527122335492 ) ) ;
#17064 = CARTESIAN_POINT ( 'NONE',  ( -12.62672070884157804, -20.24999999999991473, 3.550922209436377042 ) ) ;
#17065 = ORIENTED_EDGE ( 'NONE', *, *, #7735, .T. ) ;
#17066 = CARTESIAN_POINT ( 'NONE',  ( 13.37893135632597819, -19.30146650553847465, 4.738802066438188909 ) ) ;
#17067 = VECTOR ( 'NONE', #3054, 1000.000000000000000 ) ;
#17068 = DIRECTION ( 'NONE',  ( 0.000000000000000000, 1.000000000000000000, -0.000000000000000000 ) ) ;
#17069 = ORIENTED_EDGE ( 'NONE', *, *, #18190, .F. ) ;
#17070 = VECTOR ( 'NONE', #3684, 1000.000000000000000 ) ;
#17071 = VECTOR ( 'NONE', #10498, 1000.000000000000114 ) ;
#17072 = ORIENTED_EDGE ( 'NONE', *, *, #20684, .F. ) ;
#17073 = PLANE ( 'NONE',  #3769 ) ;
#17074 = CARTESIAN_POINT ( 'NONE',  ( -12.65410809543883985, -18.78004118034163739, 5.517608176248461227 ) ) ;
#17075 = EDGE_CURVE ( 'NONE', #1180, #16594, #5521, .T. ) ;
#17076 = ADVANCED_FACE ( 'NONE', ( #14578 ), #9671, .T. ) ;
#17077 = LINE ( 'NONE', #19923, #5974 ) ;
#17078 = CARTESIAN_POINT ( 'NONE',  ( -13.70116456325478893, -3.778689555664588973, 5.825679699621801433 ) ) ;
#17079 = CARTESIAN_POINT ( 'NONE',  ( 14.49999999999998579, -18.49999999999999645, 4.000000000000000000 ) ) ;
#17080 = PLANE ( 'NONE',  #11543 ) ;
#17081 = CARTESIAN_POINT ( 'NONE',  ( 4.999999999999998224, 0.000000000000000000, 9.999999999999998224 ) ) ;
#17082 = DIRECTION ( 'NONE',  ( -1.000000000000000000, 0.000000000000000000, 0.000000000000000000 ) ) ;
#17083 = VECTOR ( 'NONE', #11177, 1000.000000000000000 ) ;
#17084 = CARTESIAN_POINT ( 'NONE',  ( 11.00000000000000000, -23.83493649053891517, 5.249999999999999112 ) ) ;
#17085 = CARTESIAN_POINT ( 'NONE',  ( -8.215308582316795949, -24.52099543870834708, 2.515153566944913432 ) ) ;
#17086 = CARTESIAN_POINT ( 'NONE',  ( -1.337453470010121714, -9.114917468222230923, 1.622643865078341463 ) ) ;
#17087 = ORIENTED_EDGE ( 'NONE', *, *, #4237, .F. ) ;
#17088 = CARTESIAN_POINT ( 'NONE',  ( -13.38921792038197900, -19.53199502070850357, 5.456033026503027017 ) ) ;
#17089 = CARTESIAN_POINT ( 'NONE',  ( 11.99999999999999822, -25.50000000000000355, 1.000000000000000000 ) ) ;
#17090 = ADVANCED_FACE ( 'NONE', ( #12808 ), #19206, .T. ) ;
#17091 = CARTESIAN_POINT ( 'NONE',  ( 4.746558582316795061, -21.94931252712234127, 6.000000000000001776 ) ) ;
#17092 = CARTESIAN_POINT ( 'NONE',  ( -10.75344141768317741, -21.94931252712233061, 2.499999999999999112 ) ) ;
#17093 = VERTEX_POINT ( 'NONE', #9471 ) ;
#17094 = CARTESIAN_POINT ( 'NONE',  ( 13.40322194933353828, -19.57479155865495457, 6.214283636730510096 ) ) ;
#17095 = CARTESIAN_POINT ( 'NONE',  ( 12.62562019941893432, -20.21867992933967173, 4.757612834768309540 ) ) ;
#17096 = EDGE_LOOP ( 'NONE', ( #16498, #4313, #1276, #14202, #16982, #16523 ) ) ;
#17097 = ORIENTED_EDGE ( 'NONE', *, *, #8645, .F. ) ;
#17098 = DIRECTION ( 'NONE',  ( -0.000000000000000000, -0.000000000000000000, -1.000000000000000000 ) ) ;
#17099 = ORIENTED_EDGE ( 'NONE', *, *, #20443, .T. ) ;
#17100 = DIRECTION ( 'NONE',  ( 1.000000000000000000, 0.000000000000000000, 0.000000000000000000 ) ) ;
#17101 = VECTOR ( 'NONE', #3027, 1000.000000000000000 ) ;
#17102 = CARTESIAN_POINT ( 'NONE',  ( 0.2815691515810352930, -9.114917468222230923, 2.372643865078523984 ) ) ;
#17103 = ORIENTED_EDGE ( 'NONE', *, *, #19165, .F. ) ;
#17104 = CARTESIAN_POINT ( 'NONE',  ( -15.00000000000000000, -6.000000000000000000, 1.000000000000000000 ) ) ;
#17105 = DIRECTION ( 'NONE',  ( -0.000000000000000000, 0.000000000000000000, -1.000000000000000000 ) ) ;
#17106 = FACE_OUTER_BOUND ( 'NONE', #16404, .T. ) ;
#17107 = CARTESIAN_POINT ( 'NONE',  ( 3.521144778809589315, -10.09312707791070096, 2.066482617302010105 ) ) ;
#17108 = DIRECTION ( 'NONE',  ( 1.000000000000000000, 0.000000000000000000, -0.000000000000000000 ) ) ;
#17109 = CARTESIAN_POINT ( 'NONE',  ( 13.11740841389447709, 4.616624901677048420, 5.813473370769506765 ) ) ;
#17110 = CARTESIAN_POINT ( 'NONE',  ( -10.49999999999999822, -9.999999999999992895, 2.500000000000000000 ) ) ;
#17111 = DIRECTION ( 'NONE',  ( 1.000000000000000000, 0.000000000000000000, -0.000000000000000000 ) ) ;
#17112 = CARTESIAN_POINT ( 'NONE',  ( 13.12529397354238192, 5.014845663890295846, 4.666666666666619889 ) ) ;
#17113 = CARTESIAN_POINT ( 'NONE',  ( 7.753441417683177406, -21.94931252712233061, 2.499999999999999112 ) ) ;
#17114 = CARTESIAN_POINT ( 'NONE',  ( -12.66849571425264287, -18.05346643024382303, 5.533233176248494978 ) ) ;
#17115 = CARTESIAN_POINT ( 'NONE',  ( -11.40280858231679595, -22.46490103525074034, 2.520995438708341307 ) ) ;
#17116 = VECTOR ( 'NONE', #19408, 1000.000000000000000 ) ;
#17117 = EDGE_CURVE ( 'NONE', #16861, #682, #10543, .T. ) ;
#17118 = CARTESIAN_POINT ( 'NONE',  ( -11.50344141768317741, -22.05068747287766229, 6.000000000000001776 ) ) ;
#17119 = ORIENTED_EDGE ( 'NONE', *, *, #3786, .T. ) ;
#17120 = CARTESIAN_POINT ( 'NONE',  ( 13.09300823383486900, 4.134415808666423331, 5.226944302881396887 ) ) ;
#17121 = SURFACE_SIDE_STYLE ('',( #9579 ) ) ;
#17122 = VERTEX_POINT ( 'NONE', #16165 ) ;
#17123 = CARTESIAN_POINT ( 'NONE',  ( 11.00000000000000000, -19.49999999999999645, 5.000000000000000000 ) ) ;
#17124 = EDGE_LOOP ( 'NONE', ( #13155, #15617, #657, #3519 ) ) ;
#17125 = CARTESIAN_POINT ( 'NONE',  ( 1.925499516411631973, -10.42380411186744382, 2.516177120048874283 ) ) ;
#17126 = ORIENTED_EDGE ( 'NONE', *, *, #18622, .T. ) ;
#17127 = FACE_OUTER_BOUND ( 'NONE', #19014, .T. ) ;
#17128 = VECTOR ( 'NONE', #8303, 1000.000000000000000 ) ;
#17129 = DIRECTION ( 'NONE',  ( 0.000000000000000000, 0.000000000000000000, -1.000000000000000000 ) ) ;
#17130 = CARTESIAN_POINT ( 'NONE',  ( -2.097836924194969033, -11.64739567274323129, 2.830419876579102212 ) ) ;
#17131 = CARTESIAN_POINT ( 'NONE',  ( 0.000000000000000000, 0.000000000000000000, 4.000000000000000000 ) ) ;
#17132 = CARTESIAN_POINT ( 'NONE',  ( 3.999999999999999112, -2.500000000000047518, 2.000000000000000000 ) ) ;
#17133 = LINE ( 'NONE', #10869, #18945 ) ;
#17134 = LINE ( 'NONE', #7902, #20391 ) ;
#17135 = CARTESIAN_POINT ( 'NONE',  ( 4.753441417683176518, -21.94931252712233061, 0.9999999999999978906 ) ) ;
#17136 = DIRECTION ( 'NONE',  ( 0.000000000000000000, 0.5000000000000037748, -0.8660254037844365982 ) ) ;
#17137 = CARTESIAN_POINT ( 'NONE',  ( -7.284691417683176518, -23.77099543870834353, 4.174186261275252718 ) ) ;
#17138 = CIRCLE ( 'NONE', #8134, 0.4999999999999987232 ) ;
#17139 = EDGE_LOOP ( 'NONE', ( #4488, #16074, #14671, #20076 ) ) ;
#17140 = CARTESIAN_POINT ( 'NONE',  ( 5.777808582316794173, -20.27099543870833642, 2.724438792969431589 ) ) ;
#17141 = CARTESIAN_POINT ( 'NONE',  ( 27.50000000000000355, 3.000000000000000888, 1.000000000000000000 ) ) ;
#17142 = CARTESIAN_POINT ( 'NONE',  ( -13.38795836133016870, -20.34560275282643005, 5.879540349057044146 ) ) ;
#17143 = ORIENTED_EDGE ( 'NONE', *, *, #11822, .T. ) ;
#17144 = VECTOR ( 'NONE', #3338, 1000.000000000000000 ) ;
#17145 = EDGE_CURVE ( 'NONE', #16377, #431, #17618, .T. ) ;
#17146 = CARTESIAN_POINT ( 'NONE',  ( 5.121558582316795061, -22.99999999999999645, 3.550687472877652073 ) ) ;
#17147 = CARTESIAN_POINT ( 'NONE',  ( 0.000000000000000000, 9.000000000000001776, 1.000000000000000000 ) ) ;
#17148 = ORIENTED_EDGE ( 'NONE', *, *, #17052, .T. ) ;
#17149 = ORIENTED_EDGE ( 'NONE', *, *, #10082, .F. ) ;
#17150 = CARTESIAN_POINT ( 'NONE',  ( 13.41475008041063433, -18.99262093926051520, 6.248536519197435801 ) ) ;
#17151 = CARTESIAN_POINT ( 'NONE',  ( 17.80017143803810242, 4.999999999999999112, 1.000000000000000000 ) ) ;
#17152 = ORIENTED_EDGE ( 'NONE', *, *, #2203, .F. ) ;
#17153 = DIRECTION ( 'NONE',  ( 1.000000000000000000, 0.000000000000000000, 0.000000000000000000 ) ) ;
#17154 = ADVANCED_FACE ( 'NONE', ( #3399 ), #16057, .T. ) ;
#17155 = ORIENTED_EDGE ( 'NONE', *, *, #8111, .T. ) ;
#17156 = CARTESIAN_POINT ( 'NONE',  ( -12.24655858231679240, -21.94931252712234482, 5.250000000000000888 ) ) ;
#17157 = DIRECTION ( 'NONE',  ( 0.000000000000000000, -1.000000000000000000, 0.000000000000000000 ) ) ;
#17158 = VECTOR ( 'NONE', #5495, 1000.000000000000000 ) ;
#17159 = LINE ( 'NONE', #10576, #16535 ) ;
#17160 = CARTESIAN_POINT ( 'NONE',  ( 3.436477319925839602, -9.631595465688135960, 1.947952079262935676 ) ) ;
#17161 = CARTESIAN_POINT ( 'NONE',  ( -1.437849085826860884, 0.000000000000000000, 0.000000000000000000 ) ) ;
#17162 = CARTESIAN_POINT ( 'NONE',  ( -13.09173631808601002, 4.070184063342107805, 5.250510817581989009 ) ) ;
#17163 = CARTESIAN_POINT ( 'NONE',  ( -15.50000000000000000, -22.99999999999999289, 1.000000000000000000 ) ) ;
#17164 = CARTESIAN_POINT ( 'NONE',  ( -13.37499999999998224, -20.99999999999998934, 4.291666666666699825 ) ) ;
#17165 = CARTESIAN_POINT ( 'NONE',  ( 7.499999999999999112, -20.16506350946107418, 5.000000000000000000 ) ) ;
#17166 = CARTESIAN_POINT ( 'NONE',  ( 5.402808582316795949, -22.46490103525074034, 2.520995438708341307 ) ) ;
#17167 = VECTOR ( 'NONE', #10500, 1000.000000000000000 ) ;
#17168 = EDGE_CURVE ( 'NONE', #6657, #1638, #1730, .T. ) ;
#17169 = CARTESIAN_POINT ( 'NONE',  ( 9.440941417683177406, -21.25705176302044208, 2.828734674606458555 ) ) ;
#17170 = CARTESIAN_POINT ( 'NONE',  ( -5.496558582316794173, -22.05068747287764452, 1.749999999999998446 ) ) ;
#17171 = ORIENTED_EDGE ( 'NONE', *, *, #11899, .T. ) ;
#17172 = CARTESIAN_POINT ( 'NONE',  ( 13.09553549038190567, 4.262042264285192950, 5.042530537310905281 ) ) ;
#17173 = CARTESIAN_POINT ( 'NONE',  ( -1.852280067228949445, -9.126254559850970338, 1.625555456689752321 ) ) ;
#17174 = ORIENTED_EDGE ( 'NONE', *, *, #19240, .T. ) ;
#17175 = ORIENTED_EDGE ( 'NONE', *, *, #19264, .T. ) ;
#17176 = CARTESIAN_POINT ( 'NONE',  ( 0.000000000000000000, 10.00000000000000000, 1.000000000000000000 ) ) ;
#17177 = CARTESIAN_POINT ( 'NONE',  ( -12.62499999999998224, -20.24999999999998934, 4.291666666666698937 ) ) ;
#17178 = CARTESIAN_POINT ( 'NONE',  ( -24.87918902992234393, 16.00000000000000000, 1.000000000000000000 ) ) ;
#17179 = CARTESIAN_POINT ( 'NONE',  ( -13.37883250981221472, -20.05645825448334563, 5.102688967256983510 ) ) ;
#17180 = LINE ( 'NONE', #5793, #18084 ) ;
#17181 = LINE ( 'NONE', #7669, #19906 ) ;
#17182 = DIRECTION ( 'NONE',  ( 1.000000000000000000, 0.000000000000000000, 0.000000000000000000 ) ) ;
#17183 = CARTESIAN_POINT ( 'NONE',  ( 15.50000000000000178, -20.99999999999999645, 1.000000000000000000 ) ) ;
#17184 = CARTESIAN_POINT ( 'NONE',  ( 17.80017143803810242, 0.000000000000000000, 0.000000000000000000 ) ) ;
#17185 = CARTESIAN_POINT ( 'NONE',  ( -12.80905858231679417, -23.80360840875935935, 1.768074502826626260 ) ) ;
#17186 = CARTESIAN_POINT ( 'NONE',  ( -2.506848361495492394, -9.459347215042898327, 1.711100304737409150 ) ) ;
#17187 = VERTEX_POINT ( 'NONE', #251 ) ;
#17188 = CARTESIAN_POINT ( 'NONE',  ( -13.39170256340046095, -19.40652054827866380, 5.481861153867630065 ) ) ;
#17189 = DIRECTION ( 'NONE',  ( -0.000000000000000000, -0.000000000000000000, -1.000000000000000000 ) ) ;
#17190 = EDGE_CURVE ( 'NONE', #17093, #6020, #6542, .T. ) ;
#17191 = CARTESIAN_POINT ( 'NONE',  ( 10.28469141768317741, -24.52099543870834708, 4.484846433055073689 ) ) ;
#17192 = CARTESIAN_POINT ( 'NONE',  ( -6.347191417683176518, -21.53509896474923835, 2.520995438708346192 ) ) ;
#17193 = ORIENTED_EDGE ( 'NONE', *, *, #4835, .F. ) ;
#17194 = ADVANCED_FACE ( 'NONE', ( #4654 ), #9367, .T. ) ;
#17195 = CARTESIAN_POINT ( 'NONE',  ( 13.37499999998404299, -20.99999999996810729, 2.793053905886972998 ) ) ;
#17196 = CARTESIAN_POINT ( 'NONE',  ( -13.49999999999998401, -18.49999999999999645, 4.000000000000000000 ) ) ;
#17197 = VERTEX_POINT ( 'NONE', #19414 ) ;
#17198 = VERTEX_POINT ( 'NONE', #11046 ) ;
#17199 = CARTESIAN_POINT ( 'NONE',  ( -12.50209451496117197, 0.000000000000000000, 1.000000000000000000 ) ) ;
#17200 = ORIENTED_EDGE ( 'NONE', *, *, #16068, .T. ) ;
#17201 = CARTESIAN_POINT ( 'NONE',  ( -13.85528666703740619, 4.004476685417483139, 5.993048563355776182 ) ) ;
#17202 = PLANE ( 'NONE',  #4462 ) ;
#17203 = ORIENTED_EDGE ( 'NONE', *, *, #14111, .T. ) ;
#17204 = LINE ( 'NONE', #2881, #9526 ) ;
#17205 = FACE_OUTER_BOUND ( 'NONE', #1077, .T. ) ;
#17206 = PLANE ( 'NONE',  #13995 ) ;
#17207 = CARTESIAN_POINT ( 'NONE',  ( 1.731569788986178304, -8.364930642962441709, 1.622647248614820015 ) ) ;
#17208 = FACE_OUTER_BOUND ( 'NONE', #3670, .T. ) ;
#17209 = CARTESIAN_POINT ( 'NONE',  ( 13.12424783836753228, 4.962015837561366993, 5.328858059679200565 ) ) ;
#17210 = FACE_OUTER_BOUND ( 'NONE', #12542, .T. ) ;
#17211 = CARTESIAN_POINT ( 'NONE',  ( -22.06633994409548194, 16.00000000000000000, 1.000000000000000000 ) ) ;
#17212 = CARTESIAN_POINT ( 'NONE',  ( 0.000000000000000000, 9.000000000000001776, 1.000000000000000000 ) ) ;
#17213 = AXIS2_PLACEMENT_3D ( 'NONE', #1654, #17136, #2815 ) ;
#17214 = CARTESIAN_POINT ( 'NONE',  ( 8.597191417683177406, -22.46490103525075810, 4.479004561291653808 ) ) ;
#17215 = CARTESIAN_POINT ( 'NONE',  ( -13.10012427866737639, 3.743776072700027324, 6.001983176248468332 ) ) ;
#17216 = CARTESIAN_POINT ( 'NONE',  ( -11.12155858231679595, -22.99999999999999645, 3.550687472877652073 ) ) ;
#17217 = CARTESIAN_POINT ( 'NONE',  ( -12.15969141768317741, -22.67418626127524917, 1.729004561291651809 ) ) ;
#17218 = EDGE_LOOP ( 'NONE', ( #7226, #8895, #7117, #19848 ) ) ;
#17219 = EDGE_CURVE ( 'NONE', #734, #20304, #2991, .T. ) ;
#17220 = CARTESIAN_POINT ( 'NONE',  ( 13.37559048950600626, -19.47018027994350220, 4.620717101209816491 ) ) ;
#17221 = DIRECTION ( 'NONE',  ( -0.000000000000000000, -0.000000000000000000, -1.000000000000000000 ) ) ;
#17222 = ORIENTED_EDGE ( 'NONE', *, *, #12397, .T. ) ;
#17223 = DIRECTION ( 'NONE',  ( 3.469446951953619119E-16, -1.000000000000000000, 0.000000000000000000 ) ) ;
#17224 = VERTEX_POINT ( 'NONE', #7805 ) ;
#17225 = CARTESIAN_POINT ( 'NONE',  ( 2.367358971471363649, -9.400572650371021410, 2.446005822389718087 ) ) ;
#17226 = APPLICATION_CONTEXT ( 'automotive_design' ) ;
#17227 = VERTEX_POINT ( 'NONE', #14167 ) ;
#17228 = DIRECTION ( 'NONE',  ( -1.000000000000000000, 0.000000000000000000, 0.000000000000000000 ) ) ;
#17229 = EDGE_CURVE ( 'NONE', #17871, #10048, #17420, .T. ) ;
#17230 = CARTESIAN_POINT ( 'NONE',  ( 0.000000000000000000, 16.00000000000000000, 1.000000000000000000 ) ) ;
#17231 = CARTESIAN_POINT ( 'NONE',  ( -1.939860967060266672, -10.52577007527361808, 2.542364016426418516 ) ) ;
#17232 = DIRECTION ( 'NONE',  ( 1.000000000000000000, 0.000000000000000000, 0.000000000000000000 ) ) ;
#17233 = DIRECTION ( 'NONE',  ( 0.000000000000000000, -1.000000000000000000, 0.000000000000000000 ) ) ;
#17234 = CARTESIAN_POINT ( 'NONE',  ( -27.50000000000000355, 3.000000000000000888, 1.000000000000000000 ) ) ;
#17235 = CARTESIAN_POINT ( 'NONE',  ( 7.659691417683177406, -22.98484643305507191, 0.9790045612916508100 ) ) ;
#17236 = DIRECTION ( 'NONE',  ( 1.000000000000000000, 0.000000000000000000, 0.000000000000000000 ) ) ;
#17237 = CARTESIAN_POINT ( 'NONE',  ( -9.534691417683177406, -20.22900456129164581, 2.825813738724747726 ) ) ;
#17238 = ORIENTED_EDGE ( 'NONE', *, *, #15162, .T. ) ;
#17239 = CARTESIAN_POINT ( 'NONE',  ( 4.717959273841178636, -21.72818306014730183, 5.243595146365860771 ) ) ;
#17240 = DIRECTION ( 'NONE',  ( 0.000000000000000000, 1.000000000000000000, -0.000000000000000000 ) ) ;
#17241 = CARTESIAN_POINT ( 'NONE',  ( -12.65986935584910000, -19.23909752961862907, 6.257782094979345899 ) ) ;
#17242 = CARTESIAN_POINT ( 'NONE',  ( 8.684058582316794173, -20.79840458871652942, 2.226721677130544030 ) ) ;
#17243 = DIRECTION ( 'NONE',  ( 1.000000000000000000, 0.000000000000000000, 0.000000000000000000 ) ) ;
#17244 = ORIENTED_EDGE ( 'NONE', *, *, #18303, .F. ) ;
#17245 = CARTESIAN_POINT ( 'NONE',  ( 13.84997554952896515, 2.986265251207539606, 6.721192769197450012 ) ) ;
#17246 = CARTESIAN_POINT ( 'NONE',  ( -13.50000000000000178, -0.4999999999999987232, 1.000000000000000000 ) ) ;
#17247 = VERTEX_POINT ( 'NONE', #15842 ) ;
#17248 = CARTESIAN_POINT ( 'NONE',  ( 23.10856191738414012, 9.000000000000001776, 1.000000000000000000 ) ) ;
#17249 = VERTEX_POINT ( 'NONE', #7900 ) ;
#17250 = CARTESIAN_POINT ( 'NONE',  ( -11.87155858231679417, -20.24999999999999289, 3.449312527122348371 ) ) ;
#17251 = CARTESIAN_POINT ( 'NONE',  ( 12.25209451496117197, 16.00000000000000000, 1.000000000000000000 ) ) ;
#17252 = LINE ( 'NONE', #5970, #9201 ) ;
#17253 = CARTESIAN_POINT ( 'NONE',  ( 3.564229130755586006, -10.39902496812945465, 2.145043306434553987 ) ) ;
#17254 = VECTOR ( 'NONE', #662, 1000.000000000000000 ) ;
#17255 = EDGE_CURVE ( 'NONE', #3633, #19354, #1520, .T. ) ;
#17256 = FACE_OUTER_BOUND ( 'NONE', #19154, .T. ) ;
#17257 = CARTESIAN_POINT ( 'NONE',  ( -13.37499999999998401, -19.49999999999998934, 2.439580858552613751 ) ) ;
#17258 = CARTESIAN_POINT ( 'NONE',  ( 7.652808582316795061, -21.22443879296942626, 5.229004561291659137 ) ) ;
#17259 = CARTESIAN_POINT ( 'NONE',  ( -13.90439771357353038, 5.734584535470497180, 4.942866369314573127 ) ) ;
#17260 = CARTESIAN_POINT ( 'NONE',  ( 4.315753587183824180, -21.65797192216094302, 4.831781436261117335 ) ) ;
#17261 = CARTESIAN_POINT ( 'NONE',  ( 8.777808582316792396, -20.27099543870833642, 2.724438792969431589 ) ) ;
#17262 = CARTESIAN_POINT ( 'NONE',  ( 6.159691417683175629, -22.36352608949543352, 2.479004561291652031 ) ) ;
#17263 = CARTESIAN_POINT ( 'NONE',  ( -5.027808582316793284, -23.72900456129165647, 4.275561207030568411 ) ) ;
#17264 = ORIENTED_EDGE ( 'NONE', *, *, #10380, .T. ) ;
#17265 = CARTESIAN_POINT ( 'NONE',  ( 13.37680511754115287, -19.40884156416817774, 4.692171866446762429 ) ) ;
#17266 = CIRCLE ( 'NONE', #3255, 0.5000000000000000000 ) ;
#17267 = CARTESIAN_POINT ( 'NONE',  ( -20.49999999999998224, -21.99999999999999645, 12.00000000000000355 ) ) ;
#17268 = ORIENTED_EDGE ( 'NONE', *, *, #12976, .T. ) ;
#17269 = ORIENTED_EDGE ( 'NONE', *, *, #2132, .T. ) ;
#17270 = DIRECTION ( 'NONE',  ( 1.000000000000000000, -0.000000000000000000, 0.000000000000000000 ) ) ;
#17271 = CARTESIAN_POINT ( 'NONE',  ( -12.62499999999999289, -20.24999999999899103, 3.700614806296627979 ) ) ;
#17272 = CARTESIAN_POINT ( 'NONE',  ( -3.343476823822036259, -9.987837386737346890, 2.789442121235767402 ) ) ;
#17273 = CARTESIAN_POINT ( 'NONE',  ( -13.77789853026076550, 0.09637577819625635367, 5.909013032956687006 ) ) ;
#17274 = ADVANCED_FACE ( 'NONE', ( #13315 ), #7160, .T. ) ;
#17275 = FACE_OUTER_BOUND ( 'NONE', #19674, .T. ) ;
#17276 = DIRECTION ( 'NONE',  ( 1.000000000000000000, 0.000000000000000000, 0.000000000000000000 ) ) ;
#17277 = LINE ( 'NONE', #3268, #15 ) ;
#17278 = CARTESIAN_POINT ( 'NONE',  ( -26.19203811574920593, 10.00000000000000000, 1.000000000000000000 ) ) ;
#17279 = CARTESIAN_POINT ( 'NONE',  ( 12.62499999999998224, -20.24999999999991829, 4.333333333333343695 ) ) ;
#17280 = CARTESIAN_POINT ( 'NONE',  ( -10.74655858231679595, -21.94931252712234127, 6.000000000000001776 ) ) ;
#17281 = CARTESIAN_POINT ( 'NONE',  ( -2.057814715640970515, -10.20705538578787852, 1.710511717200805304 ) ) ;
#17282 = EDGE_CURVE ( 'NONE', #6562, #3751, #5372, .T. ) ;
#17283 = ORIENTED_EDGE ( 'NONE', *, *, #17255, .F. ) ;
#17284 = EDGE_CURVE ( 'NONE', #19147, #15669, #6943, .T. ) ;
#17285 = CARTESIAN_POINT ( 'NONE',  ( -13.84501469867711698, 4.235742283194553259, 4.166666666666765551 ) ) ;
#17286 = CARTESIAN_POINT ( 'NONE',  ( -13.00000000000000355, 6.123233995736752477E-17, 2.000000000000000000 ) ) ;
#17287 = AXIS2_PLACEMENT_3D ( 'NONE', #8658, #12107, #15340 ) ;
#17288 = CARTESIAN_POINT ( 'NONE',  ( 6.059058582316795949, -20.19639159124062999, 5.231925497173373074 ) ) ;
#17289 = CARTESIAN_POINT ( 'NONE',  ( -12.99655858231679595, -22.05068747287764452, 2.499999999999999112 ) ) ;
#17290 = VERTEX_POINT ( 'NONE', #2033 ) ;
#17291 = CARTESIAN_POINT ( 'NONE',  ( 13.87470602645761986, 4.985154336109792972, 3.666666666666500873 ) ) ;
#17292 = FACE_OUTER_BOUND ( 'NONE', #20381, .T. ) ;
#17293 = ORIENTED_EDGE ( 'NONE', *, *, #4575, .T. ) ;
#17294 = EDGE_CURVE ( 'NONE', #8687, #13997, #8720, .T. ) ;
#17295 = VERTEX_POINT ( 'NONE', #5073 ) ;
#17296 = DIRECTION ( 'NONE',  ( 1.000000000000000000, 0.000000000000000000, 0.000000000000000000 ) ) ;
#17297 = EDGE_LOOP ( 'NONE', ( #6428, #17536, #14250, #6691 ) ) ;
#17298 = CARTESIAN_POINT ( 'NONE',  ( 0.000000000000000000, 10.00000000000000000, 1.000000000000000000 ) ) ;
#17299 = CARTESIAN_POINT ( 'NONE',  ( 1.824488249492779879, -9.124319963227819130, 2.375058613629473570 ) ) ;
#17300 = COLOUR_RGB ( '', 0.40784314, 0.44705882, 0.49803922) ;
#17301 = ORIENTED_EDGE ( 'NONE', *, *, #8511, .T. ) ;
#17302 = PLANE ( 'NONE',  #12864 ) ;
#17303 = LINE ( 'NONE', #11043, #3672 ) ;
#17304 = EDGE_CURVE ( 'NONE', #11462, #15883, #469, .T. ) ;
#17305 = DIRECTION ( 'NONE',  ( -1.000000000000000000, 0.000000000000000000, 0.000000000000000000 ) ) ;
#17306 = CARTESIAN_POINT ( 'NONE',  ( 0.000000000000000000, -8.364917468222230923, 1.622643865078341241 ) ) ;
#17307 = PLANE ( 'NONE',  #6528 ) ;
#17308 = CARTESIAN_POINT ( 'NONE',  ( 13.12529397354238192, 5.014845663890295846, 4.166666666666765551 ) ) ;
#17309 = DIRECTION ( 'NONE',  ( -0.000000000000000000, -0.000000000000000000, -1.000000000000000000 ) ) ;
#17310 = CARTESIAN_POINT ( 'NONE',  ( -2.981555974335140152E-16, 2.500000000000002220, 1.500000000000000000 ) ) ;
#17311 = CARTESIAN_POINT ( 'NONE',  ( -9.000000000000000000, -9.999999999999992895, 2.000000000000000000 ) ) ;
#17312 = CARTESIAN_POINT ( 'NONE',  ( 5.503441417683177406, -22.05068747287766229, 4.499999999999999112 ) ) ;
#17313 = CARTESIAN_POINT ( 'NONE',  ( -12.74043380832193684, -14.42059267975384529, 5.611358176248560703 ) ) ;
#17314 = CARTESIAN_POINT ( 'NONE',  ( -7.465308582316796837, -20.97900456129165647, 3.863526089495444626 ) ) ;
#17315 = CARTESIAN_POINT ( 'NONE',  ( -10.75344141768317741, -21.94931252712233061, 1.749999999999998446 ) ) ;
#17316 = AXIS2_PLACEMENT_3D ( 'NONE', #15510, #18769, #2862 ) ;
#17317 = ORIENTED_EDGE ( 'NONE', *, *, #13846, .T. ) ;
#17318 = CARTESIAN_POINT ( 'NONE',  ( 12.99447614883396973, -0.8414544838704021146, 5.153345106674984244 ) ) ;
#17319 = DIRECTION ( 'NONE',  ( -0.000000000000000000, -0.000000000000000000, -1.000000000000000000 ) ) ;
#17320 = ORIENTED_EDGE ( 'NONE', *, *, #9473, .T. ) ;
#17321 = VECTOR ( 'NONE', #15651, 1000.000000000000000 ) ;
#17322 = ADVANCED_FACE ( 'NONE', ( #17928 ), #13421, .T. ) ;
#17323 = LINE ( 'NONE', #1639, #1950 ) ;
#17324 = ORIENTED_EDGE ( 'NONE', *, *, #19763, .T. ) ;
#17325 = CARTESIAN_POINT ( 'NONE',  ( 2.616536356806028696, -10.07836329504444706, 2.620076000170431296 ) ) ;
#17326 = AXIS2_PLACEMENT_3D ( 'NONE', #18379, #4142, #10525 ) ;
#17327 = AXIS2_PLACEMENT_3D ( 'NONE', #9901, #1953, #12927 ) ;
#17328 = EDGE_LOOP ( 'NONE', ( #1946, #9529, #3232, #18545 ) ) ;
#17329 = CARTESIAN_POINT ( 'NONE',  ( 11.40969141768317918, -21.32581373872474373, 5.270995438708348857 ) ) ;
#17330 = CARTESIAN_POINT ( 'NONE',  ( -4.000000000000000000, -8.500000000000000000, 2.392927049865408495 ) ) ;
#17331 = EDGE_CURVE ( 'NONE', #13057, #18061, #11646, .T. ) ;
#17332 = VECTOR ( 'NONE', #20514, 1000.000000000000000 ) ;
#17333 = EDGE_CURVE ( 'NONE', #11889, #6051, #16260, .T. ) ;
#17334 = CARTESIAN_POINT ( 'NONE',  ( -0.2815691515810352374, -9.864917468222230923, 1.622643865078524428 ) ) ;
#17335 = DIRECTION ( 'NONE',  ( 0.000000000000000000, 1.000000000000000000, 0.000000000000000000 ) ) ;
#17336 = CARTESIAN_POINT ( 'NONE',  ( -2.499999999999998668, -19.50000000000000000, 1.000000000000000000 ) ) ;
#17337 = VECTOR ( 'NONE', #11167, 1000.000000000000000 ) ;
#17338 = CARTESIAN_POINT ( 'NONE',  ( 12.00000000000000178, -18.50000000000000355, 4.000000000000000000 ) ) ;
#17339 = CARTESIAN_POINT ( 'NONE',  ( 8.128441417683177406, -19.49999999999998934, 3.550687472877664952 ) ) ;
#17340 = CARTESIAN_POINT ( 'NONE',  ( 0.000000000000000000, 0.000000000000000000, 1.000000000000000000 ) ) ;
#17341 = CARTESIAN_POINT ( 'NONE',  ( -7.565941417683176518, -23.20159541128344927, 2.226721677130534705 ) ) ;
#17342 = ORIENTED_EDGE ( 'NONE', *, *, #8352, .F. ) ;
#17343 = CARTESIAN_POINT ( 'NONE',  ( 5.965308582316793284, -20.22900456129164937, 4.174186261275266929 ) ) ;
#17344 = CARTESIAN_POINT ( 'NONE',  ( -13.50000000000000178, 0.000000000000000000, 2.000000000000000000 ) ) ;
#17345 = CARTESIAN_POINT ( 'NONE',  ( -13.90439735423812273, 5.734566389025032684, 4.666666666666618113 ) ) ;
#17346 = AXIS2_PLACEMENT_3D ( 'NONE', #15197, #20447, #4216 ) ;
#17347 = VERTEX_POINT ( 'NONE', #10287 ) ;
#17348 = ADVANCED_FACE ( 'NONE', ( #3705 ), #19716, .F. ) ;
#17349 = CARTESIAN_POINT ( 'NONE',  ( 9.340308582316794173, -22.67418626127525982, 5.270995438708342640 ) ) ;
#17350 = DIRECTION ( 'NONE',  ( -1.000000000000000000, -2.312964634635756072E-15, 0.000000000000000000 ) ) ;
#17351 = ORIENTED_EDGE ( 'NONE', *, *, #970, .F. ) ;
#17352 = DIRECTION ( 'NONE',  ( -0.000000000000000000, -0.000000000000000000, -1.000000000000000000 ) ) ;
#17353 =( LENGTH_UNIT ( ) NAMED_UNIT ( * ) SI_UNIT ( .MILLI., .METRE. ) );
#17354 = ORIENTED_EDGE ( 'NONE', *, *, #16387, .T. ) ;
#17355 = CARTESIAN_POINT ( 'NONE',  ( 0.000000000000000000, 0.000000000000000000, 4.000000000000000000 ) ) ;
#17356 = VERTEX_POINT ( 'NONE', #16462 ) ;
#17357 = CARTESIAN_POINT ( 'NONE',  ( -8.871558582316794173, -20.24999999999999289, 3.449312527122348371 ) ) ;
#17358 = DIRECTION ( 'NONE',  ( 0.000000000000000000, 1.000000000000000000, -0.000000000000000000 ) ) ;
#17359 = CARTESIAN_POINT ( 'NONE',  ( 13.87500000000000000, 5.000000000000049738, 4.000000000000001776 ) ) ;
#17360 = CARTESIAN_POINT ( 'NONE',  ( 1.991511895312070957, -10.01421418592441448, 1.660986244685804136 ) ) ;
#17361 = COLOUR_RGB ( '', 0.31764706, 0.68627451, 0.89019608) ;
#17362 = CARTESIAN_POINT ( 'NONE',  ( 0.000000000000000000, -0.5000000000000004441, 1.000000000000000000 ) ) ;
#17363 = CARTESIAN_POINT ( 'NONE',  ( -13.08559773465513487, 3.760185600081874746, 5.252303440007609403 ) ) ;
#17364 = CARTESIAN_POINT ( 'NONE',  ( 5.215308582316793284, -23.77099543870833998, 2.825813738724734847 ) ) ;
#17365 = CARTESIAN_POINT ( 'NONE',  ( -12.65679946139692902, -19.39412719945235253, 6.251687395662565372 ) ) ;
#17366 = VECTOR ( 'NONE', #10553, 1000.000000000000000 ) ;
#17367 = LINE ( 'NONE', #9428, #18754 ) ;
#17368 = CARTESIAN_POINT ( 'NONE',  ( -10.43924542913431175, 10.00000000000000000, 1.000000000000000000 ) ) ;
#17369 = EDGE_CURVE ( 'NONE', #19920, #19324, #3499, .T. ) ;
#17370 = CARTESIAN_POINT ( 'NONE',  ( 5.034691417683177406, -20.97900456129164581, 3.136473910504570917 ) ) ;
#17371 = CARTESIAN_POINT ( 'NONE',  ( -10.37844141768317741, -23.74999999999999645, 3.449312527122335492 ) ) ;
#17372 = ORIENTED_EDGE ( 'NONE', *, *, #12067, .T. ) ;
#17373 = CARTESIAN_POINT ( 'NONE',  ( 13.37559048950600626, -19.47018027994350220, 4.620717101209816491 ) ) ;
#17374 = VECTOR ( 'NONE', #12316, 1000.000000000000000 ) ;
#17375 = CARTESIAN_POINT ( 'NONE',  ( -2.762374231067749708, -9.968169115173667549, 1.841775933429679268 ) ) ;
#17376 = ORIENTED_EDGE ( 'NONE', *, *, #5100, .T. ) ;
#17377 = AXIS2_PLACEMENT_3D ( 'NONE', #16921, #2706, #4170 ) ;
#17378 = PRODUCT_DEFINITION_FORMATION_WITH_SPECIFIED_SOURCE ( 'ANY', '', #1665, .NOT_KNOWN. ) ;
#17379 = VERTEX_POINT ( 'NONE', #2136 ) ;
#17380 = CARTESIAN_POINT ( 'NONE',  ( 0.000000000000000000, 4.999999999999999112, 1.000000000000000000 ) ) ;
#17381 = VECTOR ( 'NONE', #859, 1000.000000000000000 ) ;
#17382 = VECTOR ( 'NONE', #19681, 1000.000000000000000 ) ;
#17383 = CARTESIAN_POINT ( 'NONE',  ( -13.11514659413808737, 4.502403003978772134, 5.887634658581065494 ) ) ;
#17384 = CARTESIAN_POINT ( 'NONE',  ( -2.910499702382182807, -8.879427762644468203, 2.504780387061739333 ) ) ;
#17385 = CARTESIAN_POINT ( 'NONE',  ( -22.06633994409548194, 10.00000000000000000, 1.000000000000000000 ) ) ;
#17386 = FACE_OUTER_BOUND ( 'NONE', #939, .T. ) ;
#17387 = CARTESIAN_POINT ( 'NONE',  ( 15.00000000000000355, -5.999999999999996447, 2.000000000000000000 ) ) ;
#17388 = CARTESIAN_POINT ( 'NONE',  ( 10.18405858231679417, -20.79840458871652942, 2.226721677130544030 ) ) ;
#17389 = DIRECTION ( 'NONE',  ( -1.000000000000000000, 0.000000000000000000, 0.000000000000000000 ) ) ;
#17390 = CARTESIAN_POINT ( 'NONE',  ( 12.62500000000001954, -20.25000000000274269, 4.083333333315724012 ) ) ;
#17391 = CARTESIAN_POINT ( 'NONE',  ( -5.121558582316795061, -24.50000000000000000, 3.550687472877651629 ) ) ;
#17392 = CARTESIAN_POINT ( 'NONE',  ( -1.619022621591186928, -9.864917468222230923, 1.622643865078341907 ) ) ;
#17393 = ORIENTED_EDGE ( 'NONE', *, *, #4754, .F. ) ;
#17394 = CARTESIAN_POINT ( 'NONE',  ( -13.84051394328565365, 4.008454135954084840, 5.243107695145536873 ) ) ;
#17395 = VECTOR ( 'NONE', #6213, 1000.000000000000000 ) ;
#17396 = CARTESIAN_POINT ( 'NONE',  ( 15.50000000000000178, -23.00000000000000711, 1.000000000000000000 ) ) ;
#17397 = VECTOR ( 'NONE', #8219, 1000.000000000000114 ) ;
#17398 = CARTESIAN_POINT ( 'NONE',  ( 6.440941417683175629, -20.19639159124061933, 1.768074502826635586 ) ) ;
#17399 = CARTESIAN_POINT ( 'NONE',  ( -12.15280858231679950, -21.53509896474924901, 4.479004561291659137 ) ) ;
#17400 = ORIENTED_EDGE ( 'NONE', *, *, #16821, .T. ) ;
#17401 = VECTOR ( 'NONE', #2113, 1000.000000000000000 ) ;
#17402 = CARTESIAN_POINT ( 'NONE',  ( 13.40653076352726103, -19.40769644187082932, 6.236886054669082746 ) ) ;
#17403 = VECTOR ( 'NONE', #19323, 1000.000000000000000 ) ;
#17404 = CARTESIAN_POINT ( 'NONE',  ( 12.62503117662529739, -20.24842558042254836, 4.565011198945062354 ) ) ;
#17405 = CARTESIAN_POINT ( 'NONE',  ( 23.60856191738414012, 0.000000000000000000, 1.000000000000000000 ) ) ;
#17406 = ORIENTED_EDGE ( 'NONE', *, *, #784, .F. ) ;
#17407 = EDGE_CURVE ( 'NONE', #12358, #5810, #11068, .T. ) ;
#17408 = ORIENTED_EDGE ( 'NONE', *, *, #8949, .F. ) ;
#17409 = DIRECTION ( 'NONE',  ( 1.000000000000000000, 0.000000000000000000, 0.000000000000000000 ) ) ;
#17410 = FACE_OUTER_BOUND ( 'NONE', #8018, .T. ) ;
#17411 = EDGE_CURVE ( 'NONE', #13991, #9844, #14685, .T. ) ;
#17412 = EDGE_CURVE ( 'NONE', #3772, #3612, #8517, .T. ) ;
#17413 = EDGE_LOOP ( 'NONE', ( #13025, #18089, #12715, #3413 ) ) ;
#17414 = FACE_BOUND ( 'NONE', #1408, .T. ) ;
#17415 = CARTESIAN_POINT ( 'NONE',  ( 3.047379876266447685, -13.13734219723468755, 3.405682891496055742 ) ) ;
#17416 = AXIS2_PLACEMENT_3D ( 'NONE', #18971, #8091, #9339 ) ;
#17417 = AXIS2_PLACEMENT_3D ( 'NONE', #18160, #1109, #5600 ) ;
#17418 = PLANE ( 'NONE',  #9659 ) ;
#17419 = CARTESIAN_POINT ( 'NONE',  ( 2.589709240944451096, -9.559844081062008669, 1.736909907557668165 ) ) ;
#17420 = LINE ( 'NONE', #3096, #12518 ) ;
#17421 = CYLINDRICAL_SURFACE ( 'NONE', #7439, 10.00000000000000000 ) ;
#17422 = DIRECTION ( 'NONE',  ( 0.000000000000000000, -0.000000000000000000, 1.000000000000000000 ) ) ;
#17423 = CARTESIAN_POINT ( 'NONE',  ( 26.69203811574920948, 1.543443504701929706E-14, 1.000000000000000000 ) ) ;
#17424 = CARTESIAN_POINT ( 'NONE',  ( -1.717920576997000737, -9.114924032904250240, 2.372645551019823884 ) ) ;
#17425 = CARTESIAN_POINT ( 'NONE',  ( 5.972191417683178294, -22.97900456129165292, 3.035098964749240125 ) ) ;
#17426 = CARTESIAN_POINT ( 'NONE',  ( -12.66369984131459070, -18.29565801360988075, 5.528024842915327142 ) ) ;
#17427 = CARTESIAN_POINT ( 'NONE',  ( -10.27780858231679595, -21.02099543870833998, 3.035098964749253003 ) ) ;
#17428 = CARTESIAN_POINT ( 'NONE',  ( -5.784691417683178294, -24.52099543870834708, 4.484846433055073689 ) ) ;
#17429 = ORIENTED_EDGE ( 'NONE', *, *, #1493, .F. ) ;
#17430 = CARTESIAN_POINT ( 'NONE',  ( 13.09560264576187905, 4.265433610975056133, 4.333333333333380999 ) ) ;
#17431 = CARTESIAN_POINT ( 'NONE',  ( -3.999999999999999112, -2.500000000000047518, 9.999999999999998224 ) ) ;
#17432 = ORIENTED_EDGE ( 'NONE', *, *, #8787, .F. ) ;
#17433 = AXIS2_PLACEMENT_3D ( 'NONE', #12630, #19035, #4690 ) ;
#17434 = DIRECTION ( 'NONE',  ( -1.000000000000000000, -0.000000000000000000, -0.000000000000000000 ) ) ;
#17435 = EDGE_CURVE ( 'NONE', #17639, #15169, #564, .T. ) ;
#17436 = EDGE_LOOP ( 'NONE', ( #8630, #4183, #5842, #18874, #18559, #3919 ) ) ;
#17437 = DIRECTION ( 'NONE',  ( -1.000000000000000000, 0.000000000000000000, 0.000000000000000000 ) ) ;
#17438 = ORIENTED_EDGE ( 'NONE', *, *, #669, .T. ) ;
#17439 = CARTESIAN_POINT ( 'NONE',  ( 0.000000000000000000, 4.999999999999999112, 0.000000000000000000 ) ) ;
#17440 = DIRECTION ( 'NONE',  ( 0.000000000000000000, -0.9659258262890672020, 0.2588190451025245142 ) ) ;
#17441 = CARTESIAN_POINT ( 'NONE',  ( -1.824218240560544047, -9.921717538097572842, 2.387231257717697286 ) ) ;
#17442 = LINE ( 'NONE', #3121, #3021 ) ;
#17443 = CARTESIAN_POINT ( 'NONE',  ( -8.965308582316794173, -20.22900456129164937, 4.174186261275266929 ) ) ;
#17444 = AXIS2_PLACEMENT_3D ( 'NONE', #17298, #6018, #18786 ) ;
#17445 = SURFACE_SIDE_STYLE ('',( #13043 ) ) ;
#17446 = CARTESIAN_POINT ( 'NONE',  ( 4.284691417683177406, -24.52099543870834708, 4.484846433055073689 ) ) ;
#17447 = CARTESIAN_POINT ( 'NONE',  ( 19.19064177244175440, 16.00000000000000000, 1.000000000000000000 ) ) ;
#17448 = CARTESIAN_POINT ( 'NONE',  ( -9.159691417683179182, -22.67418626127524917, 1.729004561291651809 ) ) ;
#17449 = ORIENTED_EDGE ( 'NONE', *, *, #19098, .T. ) ;
#17450 = CARTESIAN_POINT ( 'NONE',  ( 8.496558582316794173, -22.05068747287764452, 1.749999999999998446 ) ) ;
#17451 = LINE ( 'NONE', #6479, #19447 ) ;
#17452 = CARTESIAN_POINT ( 'NONE',  ( -12.75496035233418013, -14.43700220713569138, 6.361037912489419632 ) ) ;
#17453 = ORIENTED_EDGE ( 'NONE', *, *, #18102, .T. ) ;
#17454 = CARTESIAN_POINT ( 'NONE',  ( 9.059058582316794173, -20.72672167713054137, 4.701595411283463477 ) ) ;
#17455 = ADVANCED_FACE ( 'NONE', ( #16358 ), #3809, .T. ) ;
#17456 = DIRECTION ( 'NONE',  ( -0.000000000000000000, 0.000000000000000000, 1.000000000000000000 ) ) ;
#17457 = EDGE_CURVE ( 'NONE', #17224, #17017, #11818, .T. ) ;
#17458 = VERTEX_POINT ( 'NONE', #11853 ) ;
#17459 = DIRECTION ( 'NONE',  ( -1.000000000000000000, -0.000000000000000000, -0.000000000000000000 ) ) ;
#17460 = ORIENTED_EDGE ( 'NONE', *, *, #4276, .T. ) ;
#17461 = VECTOR ( 'NONE', #533, 1000.000000000000000 ) ;
#17462 = ADVANCED_FACE ( 'NONE', ( #3908 ), #16971, .F. ) ;
#17463 = CARTESIAN_POINT ( 'NONE',  ( 19.73630159782011617, 9.000000000000001776, 1.000000000000000000 ) ) ;
#17464 = VERTEX_POINT ( 'NONE', #2648 ) ;
#17465 = CARTESIAN_POINT ( 'NONE',  ( -6.902808582316793284, -22.77556120703056308, 1.770995438708339975 ) ) ;
#17466 = DIRECTION ( 'NONE',  ( 1.000000000000000000, 0.000000000000000000, 0.000000000000000000 ) ) ;
#17467 = LINE ( 'NONE', #11500, #1145 ) ;
#17468 = CARTESIAN_POINT ( 'NONE',  ( 0.2815691515810352374, -9.864917468222230923, 1.622643865078524428 ) ) ;
#17469 = FACE_OUTER_BOUND ( 'NONE', #15217, .T. ) ;
#17470 = CARTESIAN_POINT ( 'NONE',  ( -13.84501469867711698, 4.235742283194553259, 4.166666666666765551 ) ) ;
#17471 = CARTESIAN_POINT ( 'NONE',  ( 6.902808582316793284, -22.77556120703056308, 1.770995438708339975 ) ) ;
#17472 = CARTESIAN_POINT ( 'NONE',  ( -12.66503773474750894, -18.97809439524806052, 6.263381662489337920 ) ) ;
#17473 = VECTOR ( 'NONE', #11719, 1000.000000000000000 ) ;
#17474 = CARTESIAN_POINT ( 'NONE',  ( -13.87499999999999467, 5.734882735235988349, 3.999999999999984901 ) ) ;
#17475 = CARTESIAN_POINT ( 'NONE',  ( -10.55905858231679595, -20.19639159124062999, 5.231925497173373074 ) ) ;
#17476 = CARTESIAN_POINT ( 'NONE',  ( 6.246558582316794173, -21.94931252712234482, 5.250000000000000888 ) ) ;
#17477 = CARTESIAN_POINT ( 'NONE',  ( 7.097191417683176518, -22.46490103525075810, 4.479004561291653808 ) ) ;
#17478 = CARTESIAN_POINT ( 'NONE',  ( -10.19094141768317563, -23.27327832286946219, 4.701595411283453707 ) ) ;
#17479 = ORIENTED_EDGE ( 'NONE', *, *, #2061, .T. ) ;
#17480 = CARTESIAN_POINT ( 'NONE',  ( 13.84051394328565365, 4.008454135954084840, 5.243107695145536873 ) ) ;
#17481 = DIRECTION ( 'NONE',  ( 1.000000000000000000, 0.000000000000000000, -0.000000000000000000 ) ) ;
#17482 = VERTEX_POINT ( 'NONE', #2539 ) ;
#17483 = VERTEX_POINT ( 'NONE', #9036 ) ;
#17484 = FACE_OUTER_BOUND ( 'NONE', #18076, .T. ) ;
#17485 = CARTESIAN_POINT ( 'NONE',  ( -13.12529397354238192, 5.014845663890295846, 4.666666666666619889 ) ) ;
#17486 = CARTESIAN_POINT ( 'NONE',  ( -1.337453470010121714, -9.114917468222230923, 2.372643865078341019 ) ) ;
#17487 = CARTESIAN_POINT ( 'NONE',  ( 1.548630333695928396, -9.114917468222230923, 2.372643865078341019 ) ) ;
#17488 = ADVANCED_FACE ( 'NONE', ( #12263 ), #16869, .T. ) ;
#17489 = LINE ( 'NONE', #11217, #15351 ) ;
#17490 = CARTESIAN_POINT ( 'NONE',  ( -12.68288333306630378, -17.32689168014509207, 5.548858176248425700 ) ) ;
#17491 = CARTESIAN_POINT ( 'NONE',  ( 10.93405858231679417, -23.20159541128345992, 4.773278322869455970 ) ) ;
#17492 = FACE_OUTER_BOUND ( 'NONE', #1869, .T. ) ;
#17493 = CARTESIAN_POINT ( 'NONE',  ( 12.67822638532683577, -18.31206754099172684, 6.277704579156187847 ) ) ;
#17494 = CARTESIAN_POINT ( 'NONE',  ( -1.126276606324276619, -9.864917468222230923, 1.622643865078341907 ) ) ;
#17495 = ORIENTED_EDGE ( 'NONE', *, *, #11235, .T. ) ;
#17496 = CARTESIAN_POINT ( 'NONE',  ( -13.87470602645415063, 4.985154336109792972, 3.333333333332063830 ) ) ;
#17497 = DIRECTION ( 'NONE',  ( -0.000000000000000000, -0.000000000000000000, -1.000000000000000000 ) ) ;
#17498 = CARTESIAN_POINT ( 'NONE',  ( 6.253441417683175629, -21.94931252712233061, 0.9999999999999978906 ) ) ;
#17499 = CARTESIAN_POINT ( 'NONE',  ( -6.440941417683175629, -21.25705176302044208, 2.828734674606458555 ) ) ;
#17500 = ORIENTED_EDGE ( 'NONE', *, *, #17331, .T. ) ;
#17501 = CARTESIAN_POINT ( 'NONE',  ( 13.37499999999998401, -20.99999999999999645, 3.666666666666654084 ) ) ;
#17502 = CARTESIAN_POINT ( 'NONE',  ( 12.62499999999998224, -20.24999999999998934, 4.291666666666698937 ) ) ;
#17503 = DIRECTION ( 'NONE',  ( 0.000000000000000000, 0.000000000000000000, 1.000000000000000000 ) ) ;
#17504 = ORIENTED_EDGE ( 'NONE', *, *, #17255, .T. ) ;
#17505 = EDGE_LOOP ( 'NONE', ( #18357, #17393, #11630, #3007 ) ) ;
#17506 = CARTESIAN_POINT ( 'NONE',  ( 0.000000000000000000, 16.00000000000000000, 1.000000000000000000 ) ) ;
#17507 = CARTESIAN_POINT ( 'NONE',  ( -20.00000000000000000, 3.499999999999999556, 1.000000000000000000 ) ) ;
#17508 = PLANE ( 'NONE',  #12649 ) ;
#17509 = LINE ( 'NONE', #4457, #20710 ) ;
#17510 =( BOUNDED_SURFACE ( )  B_SPLINE_SURFACE ( 3, 2, ( 
 ( #12543, #9311, #9005, #18840, #13905, #20305, #4191, #12447, #2615, #12342, #16941, #7750, #17156, #15378, #4504, #9417, #17250, #10987, #2728, #947, #7334, #14115, #20417, #5967, #10787, #13697, #7442, #5868, #20104, #10888, #2833, #6174, #18736, #9111, #18630, #4402, #1264, #18940, #2931, #5767, #12138, #7640, #6078, #15686, #4595, #1369, #18529, #10677, #17357, #13803, #3040, #20208, #12237, #4293, #17050, #19462, #11093, #20618, #3546, #12642, #6491, #17778, #16716, #3445, #14528, #203, #6385, #5012, #9513, #17465, #307, #12751, #8057, #19155, #4810, #15789, #1467, #11189, #17564, #8259, #14208, #3141, #12852, #17878, #11284, #1775, #6269, #3342, #3237, #8162, #9824, #9609, #19254, #6587, #15993 ),
 ( #11497, #19048, #11393, #1564, #14421, #7941, #17668, #14624, #1671, #15886, #105, #4906, #12952, #19355, #14311, #16209, #9721, #16105, #1876, #6692, #5118, #13062, #7846, #4702, #2166, #8070, #14434, #10014, #116, #6502, #17475, #5513, #1684, #12862, #10219, #15896, #19167, #14822, #19860, #13246, #3741, #7950, #5303, #19266, #10122, #5413, #4918, #497, #16494, #11295, #2264, #19644, #15025, #13457, #9, #6984, #3247, #16392, #9621, #11677, #16587, #17683, #4821, #3632, #2071, #8455, #6877, #18075, #1576, #16005, #8550, #14920, #19753, #12762, #598, #13353, #11785, #18177, #3839, #3153, #9524, #8653, #11200, #706, #7092, #17575, #14324, #6397, #18491, #15135, #2687, #13556, #2575, #810, #18696 ),
 ( #5616, #16696, #4153, #13768, #9172, #2374, #7507, #8764, #9074, #11991, #20066, #12102, #17118, #12300, #18389, #8960, #13656, #15547, #3939, #1016, #10535, #10327, #19957, #4363, #1227, #10746, #7193, #2798, #7292, #13870, #4052, #16905, #4254, #10436, #15335, #16805, #13969, #7406, #12200, #18277, #20171, #7603, #5731, #2473, #907, #5831, #18590, #10633, #17010, #8865, #15233, #15445, #1129, #20270, #5928, #20375, #11885, #19008, #17524, #6235, #14490, #8124, #9376, #20485, #17628, #14384, #14076, #3205, #12605, #4664, #9271, #9576, #7709, #17428, #15644, #12817, #1530, #6140, #15950, #6037, #1631, #16069, #7813, #12409, #18804, #19217, #4770, #20583, #15851, #4470, #12510, #10949, #10854, #8013, #7910 ),
 ( #3001, #14175, #6344, #3301, #67, #17217, #2895, #12714, #14273, #9481, #4870, #19117, #1332, #15751, #11249, #18907, #20681, #4564, #11155, #11055, #17315, #9683, #1433, #3106, #6454, #1741, #11558, #2146, #5083, #8527, #19621, #5279, #11461, #6761, #19427, #11655, #17843, #3508, #13130, #9889, #16269, #167, #8629, #1938, #8321, #13327, #19317, #1839, #17939, #2242, #16370, #6854, #11354, #8433, #14696, #13224, #14898, #377, #3607, #18049, #19527, #5388, #2048, #18154, #16566, #3408, #10097, #6653, #5180, #13024, #14802, #479, #11762, #3719, #6551, #12914, #16473, #575, #9989, #19727, #6955, #4973, #3818, #10197, #9790, #17743, #16175, #8224, #14588, #262, #18666, #10299, #19837, #2769, #11862 ),
 ( #16981, #13741, #20144, #5594, #885, #13534, #5804, #11964, #18362, #7270, #4025, #10409, #14999, #681, #19936, #16781, #7480, #13432, #16670, #12075, #17092, #10509, #989, #5489, #2550, #2449, #7378, #2658, #8842, #18466, #12175, #15209, #20244, #16880, #12274, #10719, #18256, #4228, #786, #13631, #7171, #8937, #13841, #20039, #2347, #5703, #4128, #15308, #18563, #10608, #3918, #9048, #15417, #1101, #5902, #8740, #4335, #7067, #15109, #20654, #9347, #17603, #11227, #12486, #2869, #41, #17499, #17192, #6311, #15726, #1407, #12384, #12686, #10827, #20559, #18777, #15926, #4636, #9246, #19088, #9148, #4743, #19193, #10924, #15517, #1202, #1603, #7886, #2971, #18981, #7578, #15616, #14049, #13941, #11130 ),
 ( #20343, #11029, #4444, #6007, #17289, #4846, #14152, #6210, #1299, #3179, #7680, #20458, #7789, #17399, #6427, #6115, #9553, #18878, #7982, #4539, #12580, #3081, #14355, #12791, #9455, #15827, #1504, #14245, #16040, #13102, #16246, #1716, #11327, #10074, #550, #16448, #19295, #8503, #19399, #19599, #12891, #9862, #16344, #8101, #8296, #14465, #5361, #1915, #3581, #9654, #19505, #2019, #8409, #17714, #11629, #5156, #14670, #3385, #18019, #6930, #6737, #17819, #6831, #14776, #350, #8200, #11535, #453, #4948, #11435, #144, #9764, #3690, #13297, #19698, #6530, #2122, #17914, #9962, #3486, #16150, #13200, #1814, #6628, #5252, #5058, #14566, #14874, #11739, #239, #12997, #3276, #7245, #18334, #961 ),
 ( #2426, #7039, #13607, #5675, #4103, #3997, #16954, #11938, #3893, #18131, #8915, #5880, #10486, #5781, #1076, #9020, #10382, #7455, #15080, #7350, #19913, #13712, #762, #12046, #2219, #18441, #13511, #19813, #5567, #18230, #2523, #16543, #10272, #20011, #10586, #16755, #5467, #7147, #8817, #15185, #862, #16856, #8602, #16640, #15283, #20118, #12150, #13408, #18541, #4204, #2633, #15391, #13817, #3796, #20219, #10173, #11839, #14973, #651, #2320, #8708, #18855, #4516, #15492, #3057, #13917, #2942, #1176, #19060, #7764, #20319, #9431, #12, #7860, #1579, #14025, #12250, #18642, #4718, #11002, #6093, #1383, #4308, #5982, #17170, #10693, #15803, #14129, #11107, #17263, #20434, #9221, #12461, #12555, #3156 ) ),
 .UNSPECIFIED., .T., .F., .F. ) 
 B_SPLINE_SURFACE_WITH_KNOTS ( ( 4, 3, 4 ),
 ( 3, 2, 2, 2, 2, 2, 2, 2, 2, 2, 2, 2, 2, 2, 2, 2, 2, 2, 2, 2, 2, 2, 2, 2, 2, 2, 2, 2, 2, 2, 2, 2, 2, 2, 2, 2, 2, 2, 2, 2, 2, 2, 2, 2, 2, 2, 2, 3 ),
 ( 0.000000000000000000, 0.5000000000000000000, 1.000000000000000000 ),
 ( 0.000000000000000000, 0.02083333333333333218, 0.04166666666666666435, 0.06250000000000000000, 0.08333333333333332871, 0.1041666666666666713, 0.1250000000000000000, 0.1458333333333333426, 0.1666666666666666574, 0.1875000000000000000, 0.2083333333333333426, 0.2291666666666666574, 0.2500000000000000000, 0.2708333333333333148, 0.2916666666666666852, 0.3125000000000000000, 0.3333333333333333148, 0.3541666666666666852, 0.3750000000000000000, 0.3958333333333333148, 0.4166666666666666852, 0.4375000000000000000, 0.4583333333333333148, 0.4791666666666666852, 0.5000000000000000000, 0.5208333333333333703, 0.5416666666666666297, 0.5625000000000000000, 0.5833333333333333703, 0.6041666666666666297, 0.6250000000000000000, 0.6458333333333333703, 0.6666666666666666297, 0.6875000000000000000, 0.7083333333333333703, 0.7291666666666666297, 0.7500000000000000000, 0.7708333333333333703, 0.7916666666666666297, 0.8125000000000000000, 0.8333333333333333703, 0.8541666666666666297, 0.8750000000000000000, 0.8958333333333333703, 0.9166666666666666297, 0.9375000000000000000, 0.9583333333333333703, 0.9650437087885355147 ),
 .UNSPECIFIED. ) 
 GEOMETRIC_REPRESENTATION_ITEM ( )  RATIONAL_B_SPLINE_SURFACE ( (
 ( 1.000000000000000000, 0.9238795325112867385, 1.000000000000000000, 0.9238795325112867385, 1.000000000000000000, 0.9238795325112867385, 1.000000000000000000, 0.9238795325112867385, 1.000000000000000000, 0.9238795325112867385, 1.000000000000000000, 0.9238795325112867385, 1.000000000000000000, 0.9238795325112867385, 1.000000000000000000, 0.9238795325112867385, 1.000000000000000000, 0.9238795325112867385, 1.000000000000000000, 0.9238795325112867385, 1.000000000000000000, 0.9238795325112867385, 1.000000000000000000, 0.9238795325112867385, 1.000000000000000000, 0.9238795325112867385, 1.000000000000000000, 0.9238795325112867385, 1.000000000000000000, 0.9238795325112867385, 1.000000000000000000, 0.9238795325112867385, 1.000000000000000000, 0.9238795325112867385, 1.000000000000000000, 0.9238795325112867385, 1.000000000000000000, 0.9238795325112867385, 1.000000000000000000, 0.9238795325112867385, 1.000000000000000000, 0.9238795325112867385, 1.000000000000000000, 0.9238795325112867385, 1.000000000000000000, 0.9238795325112867385, 1.000000000000000000, 0.9238795325112867385, 1.000000000000000000, 0.9238795325112867385, 1.000000000000000000, 0.9238795325112867385, 1.000000000000000000, 0.9238795325112867385, 1.000000000000000000, 0.9238795325112867385, 1.000000000000000000, 0.9238795325112867385, 1.000000000000000000, 0.9238795325112867385, 1.000000000000000000, 0.9238795325112867385, 1.000000000000000000, 0.9238795325112867385, 1.000000000000000000, 0.9238795325112867385, 1.000000000000000000, 0.9238795325112867385, 1.000000000000000000, 0.9238795325112867385, 1.000000000000000000, 0.9238795325112867385, 1.000000000000000000, 0.9238795325112867385, 1.000000000000000000, 0.9238795325112867385, 1.000000000000000000, 0.9238795325112867385, 1.000000000000000000, 0.9238795325112867385, 1.000000000000000000, 0.9238795325112867385, 1.000000000000000000, 0.9238795325112867385, 1.000000000000000000, 0.9238795325112867385, 1.000000000000000000, 0.9238795325112867385, 1.000000000000000000, 0.9238795325112867385, 1.000000000000000000, 0.9238795325112867385, 1.000000000000000000, 0.9754817479996107377, 0.9667580569362973497),
 ( 0.3333333333333333703, 0.3079598441704289313, 0.3333333333333333703, 0.3079598441704289313, 0.3333333333333333703, 0.3079598441704289313, 0.3333333333333333703, 0.3079598441704289313, 0.3333333333333333703, 0.3079598441704289313, 0.3333333333333333703, 0.3079598441704289313, 0.3333333333333333703, 0.3079598441704289313, 0.3333333333333333703, 0.3079598441704289313, 0.3333333333333333703, 0.3079598441704289313, 0.3333333333333333703, 0.3079598441704289313, 0.3333333333333333703, 0.3079598441704289313, 0.3333333333333333703, 0.3079598441704289313, 0.3333333333333333703, 0.3079598441704289313, 0.3333333333333333703, 0.3079598441704289313, 0.3333333333333333703, 0.3079598441704289313, 0.3333333333333333703, 0.3079598441704289313, 0.3333333333333333703, 0.3079598441704289313, 0.3333333333333333703, 0.3079598441704289313, 0.3333333333333333703, 0.3079598441704289313, 0.3333333333333333703, 0.3079598441704289313, 0.3333333333333333703, 0.3079598441704289313, 0.3333333333333333703, 0.3079598441704289313, 0.3333333333333333703, 0.3079598441704289313, 0.3333333333333333703, 0.3079598441704289313, 0.3333333333333333703, 0.3079598441704289313, 0.3333333333333333703, 0.3079598441704289313, 0.3333333333333333703, 0.3079598441704289313, 0.3333333333333333703, 0.3079598441704289313, 0.3333333333333333703, 0.3079598441704289313, 0.3333333333333333703, 0.3079598441704289313, 0.3333333333333333703, 0.3079598441704289313, 0.3333333333333333703, 0.3079598441704289313, 0.3333333333333333703, 0.3079598441704289313, 0.3333333333333333703, 0.3079598441704289313, 0.3333333333333333703, 0.3079598441704289313, 0.3333333333333333703, 0.3079598441704289313, 0.3333333333333333703, 0.3079598441704289313, 0.3333333333333333703, 0.3079598441704289313, 0.3333333333333333703, 0.3079598441704289313, 0.3333333333333333703, 0.3079598441704289313, 0.3333333333333333703, 0.3079598441704289313, 0.3333333333333333703, 0.3079598441704289313, 0.3333333333333333703, 0.3079598441704289313, 0.3333333333333333703, 0.3079598441704289313, 0.3333333333333333703, 0.3079598441704289313, 0.3333333333333333703, 0.3079598441704289313, 0.3333333333333333703, 0.3251605826665369681, 0.3222526856454325239),
 ( 0.3333333333333333703, 0.3079598441704289313, 0.3333333333333333703, 0.3079598441704289313, 0.3333333333333333703, 0.3079598441704289313, 0.3333333333333333703, 0.3079598441704289313, 0.3333333333333333703, 0.3079598441704289313, 0.3333333333333333703, 0.3079598441704289313, 0.3333333333333333703, 0.3079598441704289313, 0.3333333333333333703, 0.3079598441704289313, 0.3333333333333333703, 0.3079598441704289313, 0.3333333333333333703, 0.3079598441704289313, 0.3333333333333333703, 0.3079598441704289313, 0.3333333333333333703, 0.3079598441704289313, 0.3333333333333333703, 0.3079598441704289313, 0.3333333333333333703, 0.3079598441704289313, 0.3333333333333333703, 0.3079598441704289313, 0.3333333333333333703, 0.3079598441704289313, 0.3333333333333333703, 0.3079598441704289313, 0.3333333333333333703, 0.3079598441704289313, 0.3333333333333333703, 0.3079598441704289313, 0.3333333333333333703, 0.3079598441704289313, 0.3333333333333333703, 0.3079598441704289313, 0.3333333333333333703, 0.3079598441704289313, 0.3333333333333333703, 0.3079598441704289313, 0.3333333333333333703, 0.3079598441704289313, 0.3333333333333333703, 0.3079598441704289313, 0.3333333333333333703, 0.3079598441704289313, 0.3333333333333333703, 0.3079598441704289313, 0.3333333333333333703, 0.3079598441704289313, 0.3333333333333333703, 0.3079598441704289313, 0.3333333333333333703, 0.3079598441704289313, 0.3333333333333333703, 0.3079598441704289313, 0.3333333333333333703, 0.3079598441704289313, 0.3333333333333333703, 0.3079598441704289313, 0.3333333333333333703, 0.3079598441704289313, 0.3333333333333333703, 0.3079598441704289313, 0.3333333333333333703, 0.3079598441704289313, 0.3333333333333333703, 0.3079598441704289313, 0.3333333333333333703, 0.3079598441704289313, 0.3333333333333333703, 0.3079598441704289313, 0.3333333333333333703, 0.3079598441704289313, 0.3333333333333333703, 0.3079598441704289313, 0.3333333333333333703, 0.3079598441704289313, 0.3333333333333333703, 0.3079598441704289313, 0.3333333333333333703, 0.3079598441704289313, 0.3333333333333333703, 0.3079598441704289313, 0.3333333333333333703, 0.3079598441704289313, 0.3333333333333333703, 0.3251605826665369681, 0.3222526856454325239),
 ( 1.000000000000000000, 0.9238795325112867385, 1.000000000000000000, 0.9238795325112867385, 1.000000000000000000, 0.9238795325112867385, 1.000000000000000000, 0.9238795325112867385, 1.000000000000000000, 0.9238795325112867385, 1.000000000000000000, 0.9238795325112867385, 1.000000000000000000, 0.9238795325112867385, 1.000000000000000000, 0.9238795325112867385, 1.000000000000000000, 0.9238795325112867385, 1.000000000000000000, 0.9238795325112867385, 1.000000000000000000, 0.9238795325112867385, 1.000000000000000000, 0.9238795325112867385, 1.000000000000000000, 0.9238795325112867385, 1.000000000000000000, 0.9238795325112867385, 1.000000000000000000, 0.9238795325112867385, 1.000000000000000000, 0.9238795325112867385, 1.000000000000000000, 0.9238795325112867385, 1.000000000000000000, 0.9238795325112867385, 1.000000000000000000, 0.9238795325112867385, 1.000000000000000000, 0.9238795325112867385, 1.000000000000000000, 0.9238795325112867385, 1.000000000000000000, 0.9238795325112867385, 1.000000000000000000, 0.9238795325112867385, 1.000000000000000000, 0.9238795325112867385, 1.000000000000000000, 0.9238795325112867385, 1.000000000000000000, 0.9238795325112867385, 1.000000000000000000, 0.9238795325112867385, 1.000000000000000000, 0.9238795325112867385, 1.000000000000000000, 0.9238795325112867385, 1.000000000000000000, 0.9238795325112867385, 1.000000000000000000, 0.9238795325112867385, 1.000000000000000000, 0.9238795325112867385, 1.000000000000000000, 0.9238795325112867385, 1.000000000000000000, 0.9238795325112867385, 1.000000000000000000, 0.9238795325112867385, 1.000000000000000000, 0.9238795325112867385, 1.000000000000000000, 0.9238795325112867385, 1.000000000000000000, 0.9238795325112867385, 1.000000000000000000, 0.9238795325112867385, 1.000000000000000000, 0.9238795325112867385, 1.000000000000000000, 0.9238795325112867385, 1.000000000000000000, 0.9238795325112867385, 1.000000000000000000, 0.9238795325112867385, 1.000000000000000000, 0.9238795325112867385, 1.000000000000000000, 0.9238795325112867385, 1.000000000000000000, 0.9238795325112867385, 1.000000000000000000, 0.9754817479996107377, 0.9667580569362973497),
 ( 0.3333333333333333703, 0.3079598441704289313, 0.3333333333333333703, 0.3079598441704289313, 0.3333333333333333703, 0.3079598441704289313, 0.3333333333333333703, 0.3079598441704289313, 0.3333333333333333703, 0.3079598441704289313, 0.3333333333333333703, 0.3079598441704289313, 0.3333333333333333703, 0.3079598441704289313, 0.3333333333333333703, 0.3079598441704289313, 0.3333333333333333703, 0.3079598441704289313, 0.3333333333333333703, 0.3079598441704289313, 0.3333333333333333703, 0.3079598441704289313, 0.3333333333333333703, 0.3079598441704289313, 0.3333333333333333703, 0.3079598441704289313, 0.3333333333333333703, 0.3079598441704289313, 0.3333333333333333703, 0.3079598441704289313, 0.3333333333333333703, 0.3079598441704289313, 0.3333333333333333703, 0.3079598441704289313, 0.3333333333333333703, 0.3079598441704289313, 0.3333333333333333703, 0.3079598441704289313, 0.3333333333333333703, 0.3079598441704289313, 0.3333333333333333703, 0.3079598441704289313, 0.3333333333333333703, 0.3079598441704289313, 0.3333333333333333703, 0.3079598441704289313, 0.3333333333333333703, 0.3079598441704289313, 0.3333333333333333703, 0.3079598441704289313, 0.3333333333333333703, 0.3079598441704289313, 0.3333333333333333703, 0.3079598441704289313, 0.3333333333333333703, 0.3079598441704289313, 0.3333333333333333703, 0.3079598441704289313, 0.3333333333333333703, 0.3079598441704289313, 0.3333333333333333703, 0.3079598441704289313, 0.3333333333333333703, 0.3079598441704289313, 0.3333333333333333703, 0.3079598441704289313, 0.3333333333333333703, 0.3079598441704289313, 0.3333333333333333703, 0.3079598441704289313, 0.3333333333333333703, 0.3079598441704289313, 0.3333333333333333703, 0.3079598441704289313, 0.3333333333333333703, 0.3079598441704289313, 0.3333333333333333703, 0.3079598441704289313, 0.3333333333333333703, 0.3079598441704289313, 0.3333333333333333703, 0.3079598441704289313, 0.3333333333333333703, 0.3079598441704289313, 0.3333333333333333703, 0.3079598441704289313, 0.3333333333333333703, 0.3079598441704289313, 0.3333333333333333703, 0.3079598441704289313, 0.3333333333333333703, 0.3079598441704289313, 0.3333333333333333703, 0.3251605826665369681, 0.3222526856454325239),
 ( 0.3333333333333333703, 0.3079598441704289313, 0.3333333333333333703, 0.3079598441704289313, 0.3333333333333333703, 0.3079598441704289313, 0.3333333333333333703, 0.3079598441704289313, 0.3333333333333333703, 0.3079598441704289313, 0.3333333333333333703, 0.3079598441704289313, 0.3333333333333333703, 0.3079598441704289313, 0.3333333333333333703, 0.3079598441704289313, 0.3333333333333333703, 0.3079598441704289313, 0.3333333333333333703, 0.3079598441704289313, 0.3333333333333333703, 0.3079598441704289313, 0.3333333333333333703, 0.3079598441704289313, 0.3333333333333333703, 0.3079598441704289313, 0.3333333333333333703, 0.3079598441704289313, 0.3333333333333333703, 0.3079598441704289313, 0.3333333333333333703, 0.3079598441704289313, 0.3333333333333333703, 0.3079598441704289313, 0.3333333333333333703, 0.3079598441704289313, 0.3333333333333333703, 0.3079598441704289313, 0.3333333333333333703, 0.3079598441704289313, 0.3333333333333333703, 0.3079598441704289313, 0.3333333333333333703, 0.3079598441704289313, 0.3333333333333333703, 0.3079598441704289313, 0.3333333333333333703, 0.3079598441704289313, 0.3333333333333333703, 0.3079598441704289313, 0.3333333333333333703, 0.3079598441704289313, 0.3333333333333333703, 0.3079598441704289313, 0.3333333333333333703, 0.3079598441704289313, 0.3333333333333333703, 0.3079598441704289313, 0.3333333333333333703, 0.3079598441704289313, 0.3333333333333333703, 0.3079598441704289313, 0.3333333333333333703, 0.3079598441704289313, 0.3333333333333333703, 0.3079598441704289313, 0.3333333333333333703, 0.3079598441704289313, 0.3333333333333333703, 0.3079598441704289313, 0.3333333333333333703, 0.3079598441704289313, 0.3333333333333333703, 0.3079598441704289313, 0.3333333333333333703, 0.3079598441704289313, 0.3333333333333333703, 0.3079598441704289313, 0.3333333333333333703, 0.3079598441704289313, 0.3333333333333333703, 0.3079598441704289313, 0.3333333333333333703, 0.3079598441704289313, 0.3333333333333333703, 0.3079598441704289313, 0.3333333333333333703, 0.3079598441704289313, 0.3333333333333333703, 0.3079598441704289313, 0.3333333333333333703, 0.3079598441704289313, 0.3333333333333333703, 0.3251605826665369681, 0.3222526856454325239),
 ( 1.000000000000000000, 0.9238795325112867385, 1.000000000000000000, 0.9238795325112867385, 1.000000000000000000, 0.9238795325112867385, 1.000000000000000000, 0.9238795325112867385, 1.000000000000000000, 0.9238795325112867385, 1.000000000000000000, 0.9238795325112867385, 1.000000000000000000, 0.9238795325112867385, 1.000000000000000000, 0.9238795325112867385, 1.000000000000000000, 0.9238795325112867385, 1.000000000000000000, 0.9238795325112867385, 1.000000000000000000, 0.9238795325112867385, 1.000000000000000000, 0.9238795325112867385, 1.000000000000000000, 0.9238795325112867385, 1.000000000000000000, 0.9238795325112867385, 1.000000000000000000, 0.9238795325112867385, 1.000000000000000000, 0.9238795325112867385, 1.000000000000000000, 0.9238795325112867385, 1.000000000000000000, 0.9238795325112867385, 1.000000000000000000, 0.9238795325112867385, 1.000000000000000000, 0.9238795325112867385, 1.000000000000000000, 0.9238795325112867385, 1.000000000000000000, 0.9238795325112867385, 1.000000000000000000, 0.9238795325112867385, 1.000000000000000000, 0.9238795325112867385, 1.000000000000000000, 0.9238795325112867385, 1.000000000000000000, 0.9238795325112867385, 1.000000000000000000, 0.9238795325112867385, 1.000000000000000000, 0.9238795325112867385, 1.000000000000000000, 0.9238795325112867385, 1.000000000000000000, 0.9238795325112867385, 1.000000000000000000, 0.9238795325112867385, 1.000000000000000000, 0.9238795325112867385, 1.000000000000000000, 0.9238795325112867385, 1.000000000000000000, 0.9238795325112867385, 1.000000000000000000, 0.9238795325112867385, 1.000000000000000000, 0.9238795325112867385, 1.000000000000000000, 0.9238795325112867385, 1.000000000000000000, 0.9238795325112867385, 1.000000000000000000, 0.9238795325112867385, 1.000000000000000000, 0.9238795325112867385, 1.000000000000000000, 0.9238795325112867385, 1.000000000000000000, 0.9238795325112867385, 1.000000000000000000, 0.9238795325112867385, 1.000000000000000000, 0.9238795325112867385, 1.000000000000000000, 0.9238795325112867385, 1.000000000000000000, 0.9238795325112867385, 1.000000000000000000, 0.9754817479996107377, 0.9667580569362973497) ) ) 
 REPRESENTATION_ITEM ( '' )  SURFACE ( )  );
#17511 = DIRECTION ( 'NONE',  ( 0.000000000000000000, -1.000000000000000000, 0.000000000000000000 ) ) ;
#17512 = CARTESIAN_POINT ( 'NONE',  ( 0.5631383031621635116, -9.864917468222230923, 1.622643865078341907 ) ) ;
#17513 = CARTESIAN_POINT ( 'NONE',  ( 0.000000000000000000, 4.999999999999999112, 0.000000000000000000 ) ) ;
#17514 = CARTESIAN_POINT ( 'NONE',  ( 11.00000000000000000, -23.83493649053891517, 4.999999999999999112 ) ) ;
#17515 = EDGE_CURVE ( 'NONE', #6665, #11041, #20134, .T. ) ;
#17516 = CARTESIAN_POINT ( 'NONE',  ( -27.94203811574921659, 9.999999999999998224, 0.000000000000000000 ) ) ;
#17517 = CARTESIAN_POINT ( 'NONE',  ( 11.00000000000000000, -20.16506350946107418, 5.000000000000000000 ) ) ;
#17518 = CARTESIAN_POINT ( 'NONE',  ( -12.34030858231679240, -22.67418626127525982, 5.270995438708342640 ) ) ;
#17519 = DIRECTION ( 'NONE',  ( 1.000000000000000000, 0.000000000000000000, -0.000000000000000000 ) ) ;
#17520 = PRODUCT_DEFINITION_SHAPE ( 'NONE', 'NONE',  #20721 ) ;
#17521 = CARTESIAN_POINT ( 'NONE',  ( 4.097191417683177406, -22.46490103525075810, 4.479004561291653808 ) ) ;
#17522 = CARTESIAN_POINT ( 'NONE',  ( -13.12529397354238192, 5.014845663890295846, 4.833333333333344584 ) ) ;
#17523 = CARTESIAN_POINT ( 'NONE',  ( -11.77780858231679417, -20.27099543870833642, 2.724438792969431589 ) ) ;
#17524 = CARTESIAN_POINT ( 'NONE',  ( -7.190941417683177406, -23.80360840875937001, 5.231925497173365081 ) ) ;
#17525 = ORIENTED_EDGE ( 'NONE', *, *, #17435, .T. ) ;
#17526 = EDGE_CURVE ( 'NONE', #18629, #16327, #13621, .T. ) ;
#17527 = CARTESIAN_POINT ( 'NONE',  ( 13.37499999999998224, -19.50000000000006040, 4.416666666666682062 ) ) ;
#17528 = FILL_AREA_STYLE ('',( #11158 ) ) ;
#17529 = ORIENTED_EDGE ( 'NONE', *, *, #11895, .F. ) ;
#17530 = ADVANCED_FACE ( 'NONE', ( #8928 ), #1190, .T. ) ;
#17531 = VERTEX_POINT ( 'NONE', #7259 ) ;
#17532 = CARTESIAN_POINT ( 'NONE',  ( 27.44203811574919882, 11.64110105645932691, 10.00000000000000000 ) ) ;
#17533 = ORIENTED_EDGE ( 'NONE', *, *, #13403, .F. ) ;
#17534 = PLANE ( 'NONE',  #19135 ) ;
#17535 = ADVANCED_BREP_SHAPE_REPRESENTATION ( '', ( #17773, #18039 ), #14707 ) ;
#17536 = ORIENTED_EDGE ( 'NONE', *, *, #1802, .F. ) ;
#17537 = CARTESIAN_POINT ( 'NONE',  ( 0.000000000000000000, 9.000000000000001776, 0.000000000000000000 ) ) ;
#17538 = CARTESIAN_POINT ( 'NONE',  ( -29.44326362367960570, 13.15740888934567465, -1.641876399273490883E-15 ) ) ;
#17539 = VECTOR ( 'NONE', #4092, 1000.000000000000000 ) ;
#17540 = CARTESIAN_POINT ( 'NONE',  ( -0.5631383031621635116, -9.864917468222230923, 2.372643865078341019 ) ) ;
#17541 = LINE ( 'NONE', #7826, #20691 ) ;
#17542 = CARTESIAN_POINT ( 'NONE',  ( -11.30905858231679417, -23.27327832286945153, 2.298404588716537411 ) ) ;
#17543 = AXIS2_PLACEMENT_3D ( 'NONE', #18766, #18968, #15506 ) ;
#17544 = ADVANCED_FACE ( 'NONE', ( #7366 ), #10708, .F. ) ;
#17545 = CARTESIAN_POINT ( 'NONE',  ( 5.222191417683177406, -19.52099543870834353, 4.586221378810406257 ) ) ;
#17546 = CARTESIAN_POINT ( 'NONE',  ( 0.000000000000000000, 16.00000000000000000, 1.000000000000000000 ) ) ;
#17547 = CARTESIAN_POINT ( 'NONE',  ( -12.44094141768317741, -21.25705176302044208, 2.828734674606458555 ) ) ;
#17548 = ORIENTED_EDGE ( 'NONE', *, *, #2193, .T. ) ;
#17549 = CARTESIAN_POINT ( 'NONE',  ( 6.527808582316794173, -23.72900456129165647, 4.275561207030568411 ) ) ;
#17550 = EDGE_CURVE ( 'NONE', #18643, #6507, #4218, .T. ) ;
#17551 = LINE ( 'NONE', #6164, #14422 ) ;
#17552 = CARTESIAN_POINT ( 'NONE',  ( -12.69740987707854707, -17.34330120752609616, 6.298537912489285517 ) ) ;
#17553 = ORIENTED_EDGE ( 'NONE', *, *, #6694, .F. ) ;
#17554 = EDGE_CURVE ( 'NONE', #20304, #510, #13729, .T. ) ;
#17555 = CARTESIAN_POINT ( 'NONE',  ( 4.746558582316793284, -21.94931252712234482, 5.250000000000000888 ) ) ;
#17556 = FACE_OUTER_BOUND ( 'NONE', #741, .T. ) ;
#17557 = VERTEX_POINT ( 'NONE', #15507 ) ;
#17558 = CARTESIAN_POINT ( 'NONE',  ( 14.99999999999999645, 3.000000000000003553, 1.000000000000000000 ) ) ;
#17559 = VECTOR ( 'NONE', #4473, 1000.000000000000000 ) ;
#17560 =( NAMED_UNIT ( * ) SI_UNIT ( $, .STERADIAN. ) SOLID_ANGLE_UNIT ( ) );
#17561 = VERTEX_POINT ( 'NONE', #4013 ) ;
#17562 = CARTESIAN_POINT ( 'NONE',  ( -14.49999999999998579, -24.49999999999999289, 4.000000000000000000 ) ) ;
#17563 = EDGE_LOOP ( 'NONE', ( #3505, #18108, #2378, #16563 ) ) ;
#17564 = CARTESIAN_POINT ( 'NONE',  ( -6.059058582316793284, -20.72672167713054137, 4.701595411283463477 ) ) ;
#17565 = CARTESIAN_POINT ( 'NONE',  ( 12.64691428603184242, -19.14332855539073464, 5.509795676248469221 ) ) ;
#17566 = CARTESIAN_POINT ( 'NONE',  ( 13.92791111847407848, 9.000000000000001776, 0.000000000000000000 ) ) ;
#17567 = CARTESIAN_POINT ( 'NONE',  ( 1.407845757905374695, -9.114917468222230923, 1.622643865078341463 ) ) ;
#17568 = EDGE_CURVE ( 'NONE', #15008, #7330, #5795, .T. ) ;
#17569 = EDGE_CURVE ( 'NONE', #20470, #4209, #12165, .T. ) ;
#17570 = CARTESIAN_POINT ( 'NONE',  ( -13.81494360078803396, 10.00000000000000000, 1.000000000000000000 ) ) ;
#17571 = CARTESIAN_POINT ( 'NONE',  ( -13.84497512400090891, 4.233743762047977199, 5.032110966142367303 ) ) ;
#17572 = CARTESIAN_POINT ( 'NONE',  ( 5.684058582316794173, -20.79840458871652942, 2.226721677130544030 ) ) ;
#17573 = CARTESIAN_POINT ( 'NONE',  ( -13.90439735423812273, 5.734566389025032684, 4.666666666666618113 ) ) ;
#17574 = DIRECTION ( 'NONE',  ( -0.000000000000000000, -0.000000000000000000, -1.000000000000000000 ) ) ;
#17575 = CARTESIAN_POINT ( 'NONE',  ( -5.402808582316795949, -23.08622137881038938, 1.020995438708339309 ) ) ;
#17576 = CARTESIAN_POINT ( 'NONE',  ( 8.402808582316794173, -22.77556120703056308, 1.770995438708339975 ) ) ;
#17577 = CARTESIAN_POINT ( 'NONE',  ( 7.847191417683175629, -21.53509896474923835, 2.520995438708346192 ) ) ;
#17578 = CARTESIAN_POINT ( 'NONE',  ( -9.347191417683177406, -21.22443879296941915, 1.770995438708345748 ) ) ;
#17579 = ORIENTED_EDGE ( 'NONE', *, *, #3053, .T. ) ;
#17580 = CARTESIAN_POINT ( 'NONE',  ( 13.84501469867711698, 4.235742283194553259, 4.166666666666765551 ) ) ;
#17581 = CARTESIAN_POINT ( 'NONE',  ( 0.000000000000000000, 11.64110105645932691, 10.00000000000000000 ) ) ;
#17582 = ORIENTED_EDGE ( 'NONE', *, *, #14329, .T. ) ;
#17583 = ADVANCED_FACE ( 'NONE', ( #5582 ), #13830, .T. ) ;
#17584 = ORIENTED_EDGE ( 'NONE', *, *, #18190, .T. ) ;
#17585 = DIRECTION ( 'NONE',  ( -0.000000000000000000, -0.000000000000000000, -1.000000000000000000 ) ) ;
#17586 = AXIS2_PLACEMENT_3D ( 'NONE', #8109, #12899, #19304 ) ;
#17587 = LINE ( 'NONE', #8083, #357 ) ;
#17588 = CARTESIAN_POINT ( 'NONE',  ( -13.10821839766814279, 4.152529082241303904, 5.997503362667785609 ) ) ;
#17589 = CARTESIAN_POINT ( 'NONE',  ( -1.797604806073912709, -9.120796646272857799, 2.374153755450133740 ) ) ;
#17590 = DIRECTION ( 'NONE',  ( -0.000000000000000000, -0.000000000000000000, -1.000000000000000000 ) ) ;
#17591 = EDGE_CURVE ( 'NONE', #7736, #487, #20234, .T. ) ;
#17592 = EDGE_CURVE ( 'NONE', #13818, #17197, #4325, .T. ) ;
#17593 = DIRECTION ( 'NONE',  ( -1.000000000000000000, 0.000000000000000000, 0.000000000000000000 ) ) ;
#17594 = CARTESIAN_POINT ( 'NONE',  ( -12.62524871736568954, -20.23743977303344010, 4.661898514667671023 ) ) ;
#17595 = CARTESIAN_POINT ( 'NONE',  ( 0.000000000000000000, 4.999999999999999112, 0.000000000000000000 ) ) ;
#17596 = DIRECTION ( 'NONE',  ( 0.000000000000000000, 1.000000000000000000, 0.000000000000000000 ) ) ;
#17597 = CARTESIAN_POINT ( 'NONE',  ( 13.04271272860988340, 0.09449279482665236263, 6.673537912489449830 ) ) ;
#17598 = CARTESIAN_POINT ( 'NONE',  ( -1.837882866761050282, -9.938290523052360825, 2.391487531332776140 ) ) ;
#17599 = ORIENTED_EDGE ( 'NONE', *, *, #14288, .T. ) ;
#17600 = CARTESIAN_POINT ( 'NONE',  ( -13.87470623115321899, 4.985164673244912414, 4.958488177337359026 ) ) ;
#17601 = DIRECTION ( 'NONE',  ( 1.000000000000000000, 0.000000000000000000, 0.000000000000000000 ) ) ;
#17602 = CARTESIAN_POINT ( 'NONE',  ( 5.128441417683177406, -19.49999999999998934, 3.550687472877664952 ) ) ;
#17603 = CARTESIAN_POINT ( 'NONE',  ( -6.909691417683176518, -21.63647391050456648, 4.520995438708348857 ) ) ;
#17604 = B_SPLINE_CURVE_WITH_KNOTS ( 'NONE', 3,
 ( #8257, #14835, #507, #6888, #13258, #18678, #5815, #4454, #12185, #20357, #10933, #13851, #4346, #7799, #20154, #17299, #20469, #7491, #6126, #10729, #18989, #18890, #20254, #16993, #10839, #14059, #12495, #2984, #17102, #9158 ),
 .UNSPECIFIED., .F., .F.,
 ( 4, 2, 2, 2, 2, 2, 2, 2, 2, 2, 2, 2, 2, 2, 4 ),
 ( 0.6078525888943429045, 0.6200887121040892236, 0.6309950902025724950, 0.6419014683010558775, 0.6637142244980225314, 0.7073397368919559502, 0.7509652492858893691, 0.7727780054828560230, 0.7836843835813394055, 0.7945907616798226769, 0.8074288390748337596, 0.8202669164698448423, 0.8459430712598670077, 0.8972953808399113385, 1.000000000000000000 ),
 .UNSPECIFIED. ) ;
#17605 = EDGE_LOOP ( 'NONE', ( #15451, #9352, #16172, #8580 ) ) ;
#17606 = CARTESIAN_POINT ( 'NONE',  ( 13.90411326029870409, 5.720219645086723759, 5.230514352905474063 ) ) ;
#17607 = CARTESIAN_POINT ( 'NONE',  ( 13.00900269284621302, -0.8578640112522492034, 5.903024842915844062 ) ) ;
#17608 = PLANE ( 'NONE',  #7009 ) ;
#17609 = ORIENTED_EDGE ( 'NONE', *, *, #6410, .T. ) ;
#17610 = EDGE_CURVE ( 'NONE', #20090, #6562, #18456, .T. ) ;
#17611 = ORIENTED_EDGE ( 'NONE', *, *, #2751, .F. ) ;
#17612 = LINE ( 'NONE', #14473, #8763 ) ;
#17613 = FACE_OUTER_BOUND ( 'NONE', #7428, .T. ) ;
#17614 = AXIS2_PLACEMENT_3D ( 'NONE', #6515, #12877, #20638 ) ;
#17615 = LINE ( 'NONE', #9668, #17990 ) ;
#17616 = DIRECTION ( 'NONE',  ( 0.000000000000000000, 0.000000000000000000, 1.000000000000000000 ) ) ;
#17617 = CARTESIAN_POINT ( 'NONE',  ( 2.627360420079438263, -14.25085146736906339, 2.749039333894452763 ) ) ;
#17618 = LINE ( 'NONE', #6226, #16871 ) ;
#17619 = AXIS2_PLACEMENT_3D ( 'NONE', #19249, #4698, #14203 ) ;
#17620 = CARTESIAN_POINT ( 'NONE',  ( 0.000000000000000000, 9.000000000000001776, 1.000000000000000000 ) ) ;
#17621 = CARTESIAN_POINT ( 'NONE',  ( 20.00000000000000000, 2.500000000000004885, 1.500000000000000000 ) ) ;
#17622 = CARTESIAN_POINT ( 'NONE',  ( 0.3749999999999968914, 0.000000000000000000, 0.000000000000000000 ) ) ;
#17623 = LINE ( 'NONE', #3099, #9712 ) ;
#17624 = CARTESIAN_POINT ( 'NONE',  ( -2.579281110863027582, -9.822567596814183233, 2.554382554832406615 ) ) ;
#17625 = CARTESIAN_POINT ( 'NONE',  ( 9.059058582316795949, -21.25705176302045274, 4.171265325393551215 ) ) ;
#17626 = CARTESIAN_POINT ( 'NONE',  ( -13.08080186171710224, 3.517994016715657146, 5.247095106674282583 ) ) ;
#17627 = CARTESIAN_POINT ( 'NONE',  ( -12.52780858231679595, -23.72900456129165647, 4.275561207030568411 ) ) ;
#17628 = CARTESIAN_POINT ( 'NONE',  ( -6.628441417683177406, -19.49999999999998934, 3.550687472877664952 ) ) ;
#17629 = EDGE_LOOP ( 'NONE', ( #12079, #14411 ) ) ;
#17630 = CARTESIAN_POINT ( 'NONE',  ( 13.57153706873194032, -9.574878029060977624, 4.950999963380944280 ) ) ;
#17631 = ORIENTED_EDGE ( 'NONE', *, *, #11501, .F. ) ;
#17632 = VECTOR ( 'NONE', #4907, 1000.000000000000000 ) ;
#17633 = ORIENTED_EDGE ( 'NONE', *, *, #20543, .T. ) ;
#17634 = FACE_OUTER_BOUND ( 'NONE', #14491, .T. ) ;
#17635 = ORIENTED_EDGE ( 'NONE', *, *, #10759, .F. ) ;
#17636 = CARTESIAN_POINT ( 'NONE',  ( -21.42243175760212637, 4.999999999999999112, 0.000000000000000000 ) ) ;
#17637 = VECTOR ( 'NONE', #19759, 1000.000000000000000 ) ;
#17638 = EDGE_CURVE ( 'NONE', #18591, #11254, #20333, .T. ) ;
#17639 = VERTEX_POINT ( 'NONE', #15606 ) ;
#17640 = CARTESIAN_POINT ( 'NONE',  ( 11.12844141768317741, -20.24999999999999289, 3.550687472877664952 ) ) ;
#17641 = DIRECTION ( 'NONE',  ( 1.000000000000000000, -0.000000000000000000, -0.000000000000000000 ) ) ;
#17642 = CARTESIAN_POINT ( 'NONE',  ( -1.337453470010121714, -9.114917468222230923, 2.372643865078341019 ) ) ;
#17643 = CARTESIAN_POINT ( 'NONE',  ( 2.623717082130370137, -10.12934627674766830, 2.633169448359191644 ) ) ;
#17644 = LINE ( 'NONE', #3528, #15971 ) ;
#17645 = AXIS2_PLACEMENT_3D ( 'NONE', #18433, #1451, #5560 ) ;
#17646 = DIRECTION ( 'NONE',  ( 0.000000000000000000, -1.000000000000000000, 0.000000000000000000 ) ) ;
#17647 = CARTESIAN_POINT ( 'NONE',  ( 7.472191417683176518, -23.72900456129165292, 2.724438792969417822 ) ) ;
#17648 = DIRECTION ( 'NONE',  ( 0.000000000000000000, -1.000000000000000000, 0.000000000000000000 ) ) ;
#17649 = VECTOR ( 'NONE', #4475, 1000.000000000000000 ) ;
#17650 = CARTESIAN_POINT ( 'NONE',  ( -11.50344141768317741, -22.05068747287766229, 4.499999999999999112 ) ) ;
#17651 = ORIENTED_EDGE ( 'NONE', *, *, #5955, .T. ) ;
#17652 = CARTESIAN_POINT ( 'NONE',  ( 8.309058582316795949, -23.80360840875935935, 1.768074502826626260 ) ) ;
#17653 = DIRECTION ( 'NONE',  ( 1.000000000000000000, 0.000000000000000000, 0.000000000000000000 ) ) ;
#17654 = CARTESIAN_POINT ( 'NONE',  ( -13.90439735423812273, 5.734566389025032684, 4.333333333333380999 ) ) ;
#17655 = ORIENTED_EDGE ( 'NONE', *, *, #6466, .F. ) ;
#17656 = CARTESIAN_POINT ( 'NONE',  ( 6.246558582316794173, -21.94931252712234482, 5.250000000000000888 ) ) ;
#17657 = DIRECTION ( 'NONE',  ( 0.000000000000000000, -0.000000000000000000, 1.000000000000000000 ) ) ;
#17658 = ORIENTED_EDGE ( 'NONE', *, *, #6674, .F. ) ;
#17659 = VECTOR ( 'NONE', #13618, 1000.000000000000000 ) ;
#17660 = CARTESIAN_POINT ( 'NONE',  ( -20.75349085826862350, 11.64110105645932691, 0.000000000000000000 ) ) ;
#17661 = APPLICATION_PROTOCOL_DEFINITION ( 'draft international standard', 'automotive_design', 1998, #6262 ) ;
#17662 = VERTEX_POINT ( 'NONE', #1290 ) ;
#17663 = EDGE_CURVE ( 'NONE', #193, #17482, #16700, .T. ) ;
#17664 = VECTOR ( 'NONE', #162, 1000.000000000000000 ) ;
#17665 = DIRECTION ( 'NONE',  ( -1.000000000000000000, 0.000000000000000000, -0.000000000000000000 ) ) ;
#17666 = AXIS2_PLACEMENT_3D ( 'NONE', #8877, #4264, #18504 ) ;
#17667 = VERTEX_POINT ( 'NONE', #11219 ) ;
#17668 = CARTESIAN_POINT ( 'NONE',  ( -12.80905858231679417, -23.80360840875935935, 1.768074502826626260 ) ) ;
#17669 = FACE_OUTER_BOUND ( 'NONE', #817, .T. ) ;
#17670 = EDGE_CURVE ( 'NONE', #2072, #12804, #14040, .T. ) ;
#17671 = CARTESIAN_POINT ( 'NONE',  ( -15.00000000000000000, -6.000000000000000000, 2.000000000000000000 ) ) ;
#17672 = CARTESIAN_POINT ( 'NONE',  ( 2.155282726790247239, -12.05525952636828357, 2.935167462089139256 ) ) ;
#17673 = EDGE_CURVE ( 'NONE', #8680, #9082, #6107, .T. ) ;
#17674 = CARTESIAN_POINT ( 'NONE',  ( 12.62499999998404121, -20.24999999996810729, 2.793053905886972998 ) ) ;
#17675 = VECTOR ( 'NONE', #11670, 1000.000000000000000 ) ;
#17676 = DIRECTION ( 'NONE',  ( -0.000000000000000000, 0.000000000000000000, -1.000000000000000000 ) ) ;
#17677 = CARTESIAN_POINT ( 'NONE',  ( -13.38090111944825367, -19.20199346786276351, 4.743968713382380464 ) ) ;
#17678 = VECTOR ( 'NONE', #20361, 1000.000000000000000 ) ;
#17679 = CARTESIAN_POINT ( 'NONE',  ( 9.996558582316794173, -22.05068747287764452, 1.749999999999998446 ) ) ;
#17680 = CARTESIAN_POINT ( 'NONE',  ( -13.90439735423465351, 5.734566389025032684, 3.333333333332063386 ) ) ;
#17681 = VECTOR ( 'NONE', #5419, 1000.000000000000000 ) ;
#17682 = FACE_OUTER_BOUND ( 'NONE', #10505, .T. ) ;
#17683 = CARTESIAN_POINT ( 'NONE',  ( -7.652808582316796837, -20.91377862118960351, 5.979004561291660913 ) ) ;
#17684 = CARTESIAN_POINT ( 'NONE',  ( 8.215308582316792396, -23.77099543870833998, 2.825813738724734847 ) ) ;
#17685 = CARTESIAN_POINT ( 'NONE',  ( 6.722191417683176518, -21.02099543870834353, 3.964901035250761208 ) ) ;
#17686 = CARTESIAN_POINT ( 'NONE',  ( -8.784691417683177406, -23.77099543870834353, 4.174186261275251830 ) ) ;
#17687 = VERTEX_POINT ( 'NONE', #18869 ) ;
#17688 = ORIENTED_EDGE ( 'NONE', *, *, #9878, .F. ) ;
#17689 = CARTESIAN_POINT ( 'NONE',  ( 13.83531008031826026, 3.745659056069631898, 5.237458296715707284 ) ) ;
#17690 = FACE_OUTER_BOUND ( 'NONE', #9460, .T. ) ;
#17691 = ORIENTED_EDGE ( 'NONE', *, *, #17550, .F. ) ;
#17692 = ADVANCED_FACE ( 'NONE', ( #6520 ), #2960, .T. ) ;
#17693 = ORIENTED_EDGE ( 'NONE', *, *, #16816, .F. ) ;
#17694 = CARTESIAN_POINT ( 'NONE',  ( 21.17243175760212637, 9.000000000000001776, 0.000000000000000000 ) ) ;
#17695 = FACE_BOUND ( 'NONE', #460, .T. ) ;
#17696 = CARTESIAN_POINT ( 'NONE',  ( -13.12119116326504908, 4.807653744879115010, 5.626470997801169105 ) ) ;
#17697 = CIRCLE ( 'NONE', #990, 59.99999999999998579 ) ;
#17698 = CARTESIAN_POINT ( 'NONE',  ( -0.9854920305337621089, -9.114917468222230923, 2.372643865078341019 ) ) ;
#17699 = LINE ( 'NONE', #17385, #4673 ) ;
#17700 = VECTOR ( 'NONE', #6333, 1000.000000000000000 ) ;
#17701 = DIRECTION ( 'NONE',  ( -0.9848077530122082424, -0.1736481776669292765, 0.000000000000000000 ) ) ;
#17702 = CARTESIAN_POINT ( 'NONE',  ( -13.12270769621861355, 4.884238659038159902, 5.513847264053151065 ) ) ;
#17703 = CARTESIAN_POINT ( 'NONE',  ( 12.24655858231679240, -21.94931252712234482, 5.250000000000000888 ) ) ;
#17704 = CARTESIAN_POINT ( 'NONE',  ( 0.000000000000000000, 4.999999999999999112, 0.000000000000000000 ) ) ;
#17705 = CARTESIAN_POINT ( 'NONE',  ( 12.85087781109329974, -9.593170539812428288, 6.465204579154565145 ) ) ;
#17706 = EDGE_CURVE ( 'NONE', #3209, #20155, #17277, .T. ) ;
#17707 = CARTESIAN_POINT ( 'NONE',  ( -2.327620134574780231, -13.27885108724501251, 3.249410218619480872 ) ) ;
#17708 = AXIS2_PLACEMENT_3D ( 'NONE', #19926, #2440, #136 ) ;
#17709 = ORIENTED_EDGE ( 'NONE', *, *, #8721, .T. ) ;
#17710 = VECTOR ( 'NONE', #5633, 1000.000000000000000 ) ;
#17711 = CARTESIAN_POINT ( 'NONE',  ( -13.87470602645761986, 4.985154336109792972, 4.333333333333382775 ) ) ;
#17712 = DIRECTION ( 'NONE',  ( 0.000000000000000000, -0.000000000000000000, 1.000000000000000000 ) ) ;
#17713 = CARTESIAN_POINT ( 'NONE',  ( 6.159691417683175629, -22.98484643305507191, 0.9790045612916508100 ) ) ;
#17714 = CARTESIAN_POINT ( 'NONE',  ( -8.402808582316797725, -22.46490103525074034, 2.520995438708341307 ) ) ;
#17715 = MECHANICAL_DESIGN_GEOMETRIC_PRESENTATION_REPRESENTATION (  '', ( #17034 ), #1002 ) ;
#17716 = ORIENTED_EDGE ( 'NONE', *, *, #227, .F. ) ;
#17717 = CARTESIAN_POINT ( 'NONE',  ( 13.85956729540471066, 3.470648417939721231, 6.731609435864099211 ) ) ;
#17718 = CARTESIAN_POINT ( 'NONE',  ( 13.12529397354238192, 5.014845663890295846, 4.833333333333344584 ) ) ;
#17719 = CARTESIAN_POINT ( 'NONE',  ( -13.12500000000000533, 4.265117264764102245, 4.000000000000000888 ) ) ;
#17720 = EDGE_LOOP ( 'NONE', ( #20602, #12661, #17438, #19535 ) ) ;
#17721 = CIRCLE ( 'NONE', #8031, 10.00000000000000000 ) ;
#17722 = EDGE_CURVE ( 'NONE', #3444, #3944, #1706, .T. ) ;
#17723 = EDGE_LOOP ( 'NONE', ( #12076, #16205 ) ) ;
#17724 = EDGE_CURVE ( 'NONE', #14584, #13134, #9644, .T. ) ;
#17725 = CARTESIAN_POINT ( 'NONE',  ( 0.000000000000000000, 4.999999999999999112, 0.000000000000000000 ) ) ;
#17726 = CARTESIAN_POINT ( 'NONE',  ( -0.000000000000000000, 11.64110105645932691, 0.000000000000000000 ) ) ;
#17727 = ORIENTED_EDGE ( 'NONE', *, *, #12184, .T. ) ;
#17728 = AXIS2_PLACEMENT_3D ( 'NONE', #4901, #12947, #11280 ) ;
#17729 = CARTESIAN_POINT ( 'NONE',  ( -5.381197846483055436, -14.00000000000000000, 1.000000000000000000 ) ) ;
#17730 = CARTESIAN_POINT ( 'NONE',  ( 2.196516900615978152, -11.19187256518208784, 1.963432442569047698 ) ) ;
#17731 = DIRECTION ( 'NONE',  ( -1.000000000000000000, -0.000000000000000000, -0.000000000000000000 ) ) ;
#17732 = CARTESIAN_POINT ( 'NONE',  ( -17.11324865405191176, -11.00000000000000000, 2.000000000000000000 ) ) ;
#17733 = AXIS2_PLACEMENT_3D ( 'NONE', #19939, #13435, #10303 ) ;
#17734 = EDGE_CURVE ( 'NONE', #8562, #19322, #10557, .T. ) ;
#17735 = CIRCLE ( 'NONE', #4040, 10.00000000000000000 ) ;
#17736 = DIRECTION ( 'NONE',  ( 0.1736481776669295540, 0.9848077530122082424, 0.000000000000000000 ) ) ;
#17737 = DIRECTION ( 'NONE',  ( 0.000000000000000000, -1.000000000000000000, 0.000000000000000000 ) ) ;
#17738 = CARTESIAN_POINT ( 'NONE',  ( -12.24655858231679240, -21.94931252712234482, 5.250000000000000888 ) ) ;
#17739 = AXIS2_PLACEMENT_3D ( 'NONE', #3681, #3788, #11730 ) ;
#17740 = CARTESIAN_POINT ( 'NONE',  ( -1.824488249492779879, -9.124319963227819130, 2.375058613629473570 ) ) ;
#17741 = CARTESIAN_POINT ( 'NONE',  ( -13.09123688038123490, 4.044962459253448550, 5.255034774807352704 ) ) ;
#17742 = CARTESIAN_POINT ( 'NONE',  ( -12.24655858231679240, -21.94931252712234482, 5.250000000000000888 ) ) ;
#17743 = CARTESIAN_POINT ( 'NONE',  ( -4.659691417683178294, -22.67418626127524917, 1.729004561291651809 ) ) ;
#17744 = EDGE_LOOP ( 'NONE', ( #7175, #506, #6855, #2321 ) ) ;
#17745 = CARTESIAN_POINT ( 'NONE',  ( 13.84042474920106081, 4.003949834653575124, 5.242612001278796008 ) ) ;
#17746 = LINE ( 'NONE', #3412, #7720 ) ;
#17747 = ORIENTED_EDGE ( 'NONE', *, *, #13376, .T. ) ;
#17748 = ORIENTED_EDGE ( 'NONE', *, *, #19226, .T. ) ;
#17749 = DIRECTION ( 'NONE',  ( 0.000000000000000000, -0.000000000000000000, 1.000000000000000000 ) ) ;
#17750 = ORIENTED_EDGE ( 'NONE', *, *, #8015, .T. ) ;
#17751 = FACE_OUTER_BOUND ( 'NONE', #3871, .T. ) ;
#17752 = AXIS2_PLACEMENT_3D ( 'NONE', #9854, #2213, #14868 ) ;
#17753 = ORIENTED_EDGE ( 'NONE', *, *, #15092, .F. ) ;
#17754 = CARTESIAN_POINT ( 'NONE',  ( 9.159691417683177406, -22.67418626127524917, 1.729004561291651587 ) ) ;
#17755 = LINE ( 'NONE', #3523, #11332 ) ;
#17756 = CARTESIAN_POINT ( 'NONE',  ( -1.957016269584227031, -9.152392576945766578, 2.382268221639079364 ) ) ;
#17757 = CARTESIAN_POINT ( 'NONE',  ( 2.203959450683124377, -9.262433282444222371, 2.410528873095051594 ) ) ;
#17758 = CARTESIAN_POINT ( 'NONE',  ( -12.99655858231679417, -22.05068747287764452, 1.749999999999998446 ) ) ;
#17759 = EDGE_CURVE ( 'NONE', #17197, #4851, #18223, .T. ) ;
#17760 = DIRECTION ( 'NONE',  ( 0.000000000000000000, 1.000000000000000000, -0.000000000000000000 ) ) ;
#17761 = CARTESIAN_POINT ( 'NONE',  ( 9.253441417683177406, -21.94931252712233061, 1.749999999999998446 ) ) ;
#17762 = DIRECTION ( 'NONE',  ( 0.000000000000000000, 0.000000000000000000, 1.000000000000000000 ) ) ;
#17763 = CARTESIAN_POINT ( 'NONE',  ( -5.784691417683179182, -23.77099543870834353, 4.174186261275252718 ) ) ;
#17764 = VECTOR ( 'NONE', #2290, 1000.000000000000000 ) ;
#17765 = ORIENTED_EDGE ( 'NONE', *, *, #18314, .F. ) ;
#17766 = CARTESIAN_POINT ( 'NONE',  ( 11.87155858231679595, -19.49999999999998934, 3.449312527122348371 ) ) ;
#17767 = CARTESIAN_POINT ( 'NONE',  ( 12.64511805349267526, -19.23403829861753422, 5.507852591554869726 ) ) ;
#17768 = CARTESIAN_POINT ( 'NONE',  ( -13.15492785973632017, 5.761356916681801721, 5.116543252045025802 ) ) ;
#17769 = ORIENTED_EDGE ( 'NONE', *, *, #11352, .F. ) ;
#17770 = DIRECTION ( 'NONE',  ( 0.000000000000000000, -1.000000000000000000, 0.000000000000000000 ) ) ;
#17771 = CARTESIAN_POINT ( 'NONE',  ( 0.000000000000000000, 9.000000000000001776, 0.000000000000000000 ) ) ;
#17772 = ORIENTED_EDGE ( 'NONE', *, *, #9871, .T. ) ;
#17773 = MANIFOLD_SOLID_BREP ( 'Cut-Extrude1', #4957 ) ;
#17774 = APPLICATION_PROTOCOL_DEFINITION ( 'draft international standard', 'automotive_design', 1998, #18706 ) ;
#17775 = ORIENTED_EDGE ( 'NONE', *, *, #15526, .T. ) ;
#17776 = CARTESIAN_POINT ( 'NONE',  ( 12.74617908753018192, -19.97389846102915456, 3.534610772493881559 ) ) ;
#17777 = ORIENTED_EDGE ( 'NONE', *, *, #18619, .T. ) ;
#17778 = CARTESIAN_POINT ( 'NONE',  ( -7.652808582316795061, -21.22443879296942626, 5.229004561291659137 ) ) ;
#17779 = VECTOR ( 'NONE', #4964, 1000.000000000000000 ) ;
#17780 = CARTESIAN_POINT ( 'NONE',  ( 12.62524871736568954, -20.23743977303344010, 4.661898514667671023 ) ) ;
#17781 = CARTESIAN_POINT ( 'NONE',  ( 13.42791111847407848, 0.000000000000000000, 1.000000000000000000 ) ) ;
#17782 = CARTESIAN_POINT ( 'NONE',  ( 13.08573665985359824, 3.017201322601628100, 5.986358176248492313 ) ) ;
#17783 = DIRECTION ( 'NONE',  ( 0.000000000000000000, 0.000000000000000000, -1.000000000000000000 ) ) ;
#17784 = CARTESIAN_POINT ( 'NONE',  ( -13.84501469867711698, 4.235742283194553259, 2.999999999999999556 ) ) ;
#17785 = CARTESIAN_POINT ( 'NONE',  ( 8.684058582316795949, -20.26807450282662160, 1.696391591240633101 ) ) ;
#17786 = CARTESIAN_POINT ( 'NONE',  ( -13.15498566372047762, 5.764276017890828108, 4.942557026581394730 ) ) ;
#17787 = CARTESIAN_POINT ( 'NONE',  ( -11.87844141768317741, -24.50000000000000000, 3.449312527122335048 ) ) ;
#17788 = EDGE_CURVE ( 'NONE', #16070, #4697, #13400, .T. ) ;
#17789 = DIRECTION ( 'NONE',  ( -0.000000000000000000, 1.000000000000000000, -1.304178812473495102E-15 ) ) ;
#17790 = CARTESIAN_POINT ( 'NONE',  ( 4.068047865639282890, -21.50414067263875850, 5.566613268849052609 ) ) ;
#17791 = CIRCLE ( 'NONE', #13113, 1.499999999999996225 ) ;
#17792 = CARTESIAN_POINT ( 'NONE',  ( 8.027808582316795949, -22.97900456129165647, 3.964901035250747885 ) ) ;
#17793 = CARTESIAN_POINT ( 'NONE',  ( -6.065941417683177406, -23.20159541128344927, 2.226721677130534705 ) ) ;
#17794 = ORIENTED_EDGE ( 'NONE', *, *, #13710, .F. ) ;
#17795 = ORIENTED_EDGE ( 'NONE', *, *, #3383, .F. ) ;
#17796 = CARTESIAN_POINT ( 'NONE',  ( 13.37561105820882013, -20.21914156045197686, 4.753815841436231260 ) ) ;
#17797 = EDGE_CURVE ( 'NONE', #19731, #2846, #10374, .T. ) ;
#17798 = LINE ( 'NONE', #18674, #16162 ) ;
#17799 = DIRECTION ( 'NONE',  ( -1.000000000000000000, 0.000000000000000000, 0.000000000000000000 ) ) ;
#17800 = VERTEX_POINT ( 'NONE', #20502 ) ;
#17801 = EDGE_LOOP ( 'NONE', ( #16829, #9349, #14836, #4778 ) ) ;
#17802 = CARTESIAN_POINT ( 'NONE',  ( -19.48630159782011262, 0.000000000000000000, 1.000000000000000000 ) ) ;
#17803 = CARTESIAN_POINT ( 'NONE',  ( 19.23630159782011617, 4.999999999999999112, 0.000000000000000000 ) ) ;
#17804 = CARTESIAN_POINT ( 'NONE',  ( -13.12529380813666435, 5.014837310896125722, 5.033295791462342628 ) ) ;
#17805 = LINE ( 'NONE', #336, #19231 ) ;
#17806 = CARTESIAN_POINT ( 'NONE',  ( -3.475298211275419380, -9.785109117490691233, 1.987377451789144933 ) ) ;
#17807 = VECTOR ( 'NONE', #12445, 1000.000000000000000 ) ;
#17808 = CARTESIAN_POINT ( 'NONE',  ( 2.012076196476103362, -9.160103213191565175, 1.634248467062433541 ) ) ;
#17809 = CARTESIAN_POINT ( 'NONE',  ( -12.62499999999998224, -20.25000000000006395, 4.416666666666681174 ) ) ;
#17810 = CARTESIAN_POINT ( 'NONE',  ( 8.871558582316794173, -20.24999999999999289, 3.449312527122348371 ) ) ;
#17811 = DIRECTION ( 'NONE',  ( -0.000000000000000000, -0.000000000000000000, -1.000000000000000000 ) ) ;
#17812 = CARTESIAN_POINT ( 'NONE',  ( 12.62515553039088090, -20.24214571525854467, 4.629702272822510345 ) ) ;
#17813 = EDGE_CURVE ( 'NONE', #11889, #3716, #18549, .T. ) ;
#17814 = CYLINDRICAL_SURFACE ( 'NONE', #691, 10.00000000000000000 ) ;
#17815 = ORIENTED_EDGE ( 'NONE', *, *, #14037, .F. ) ;
#17816 = CARTESIAN_POINT ( 'NONE',  ( -13.83544900551672185, 3.002674778589386140, 5.971513032956590195 ) ) ;
#17817 = CARTESIAN_POINT ( 'NONE',  ( -1.437849085826860884, 10.00000000000000000, 1.000000000000000000 ) ) ;
#17818 = CARTESIAN_POINT ( 'NONE',  ( 4.472191417683178294, -24.47900456129165292, 2.413778621189595963 ) ) ;
#17819 = CARTESIAN_POINT ( 'NONE',  ( -7.652808582316796837, -21.53509896474924901, 4.479004561291659137 ) ) ;
#17820 = ORIENTED_EDGE ( 'NONE', *, *, #17973, .T. ) ;
#17821 = CARTESIAN_POINT ( 'NONE',  ( 13.90439735423465351, 5.734566389025032684, 3.333333333332063386 ) ) ;
#17822 = CARTESIAN_POINT ( 'NONE',  ( 13.09293046926041626, 3.380488697651010011, 5.994170676248444352 ) ) ;
#17823 = DIRECTION ( 'NONE',  ( 1.000000000000000000, 0.000000000000000000, 0.000000000000000000 ) ) ;
#17824 = ORIENTED_EDGE ( 'NONE', *, *, #4112, .F. ) ;
#17825 = ORIENTED_EDGE ( 'NONE', *, *, #13312, .T. ) ;
#17826 = FACE_OUTER_BOUND ( 'NONE', #5439, .T. ) ;
#17827 = EDGE_CURVE ( 'NONE', #3742, #13535, #17133, .T. ) ;
#17828 = DIRECTION ( 'NONE',  ( -1.000000000000000000, 0.000000000000000000, 0.000000000000000000 ) ) ;
#17829 = CARTESIAN_POINT ( 'NONE',  ( -11.00000000000000000, -20.16506350946107418, 5.250000000000000000 ) ) ;
#17830 = DIRECTION ( 'NONE',  ( 0.1351665943404306014, 0.9596796555888912339, -0.2464649070825229438 ) ) ;
#17831 = CARTESIAN_POINT ( 'NONE',  ( 2.050137595624097031, -10.15260257655714504, 1.696527147986202522 ) ) ;
#17832 = DIRECTION ( 'NONE',  ( -1.000000000000000000, 0.000000000000000000, 0.000000000000000000 ) ) ;
#17833 = CARTESIAN_POINT ( 'NONE',  ( 2.311130159782011972, 9.000000000000001776, 1.000000000000000000 ) ) ;
#17834 = EDGE_CURVE ( 'NONE', #13339, #7911, #7729, .T. ) ;
#17835 = DIRECTION ( 'NONE',  ( -1.000000000000000000, 0.000000000000000000, 0.000000000000000000 ) ) ;
#17836 = DIRECTION ( 'NONE',  ( 1.000000000000000000, 0.000000000000000000, 0.000000000000000000 ) ) ;
#17837 = CARTESIAN_POINT ( 'NONE',  ( -11.24178095869206828, 0.000000000000000000, 0.000000000000000000 ) ) ;
#17838 = EDGE_CURVE ( 'NONE', #3865, #16449, #7141, .T. ) ;
#17839 = DIRECTION ( 'NONE',  ( -0.000000000000000000, -0.000000000000000000, -1.000000000000000000 ) ) ;
#17840 = VERTEX_POINT ( 'NONE', #15073 ) ;
#17841 = CARTESIAN_POINT ( 'NONE',  ( -12.63598464672302590, -18.94527534048458151, 4.764022190007618285 ) ) ;
#17842 = CARTESIAN_POINT ( 'NONE',  ( -5.402808582316795949, -22.46490103525074034, 2.520995438708341307 ) ) ;
#17843 = CARTESIAN_POINT ( 'NONE',  ( -9.253441417683177406, -21.94931252712233061, 1.749999999999998446 ) ) ;
#17844 = VERTEX_POINT ( 'NONE', #13504 ) ;
#17845 = CARTESIAN_POINT ( 'NONE',  ( 13.84167967300649238, 4.067323486828401613, 5.231641758301140754 ) ) ;
#17846 = VECTOR ( 'NONE', #4433, 1000.000000000000000 ) ;
#17847 = CARTESIAN_POINT ( 'NONE',  ( 7.500000000000002665, -9.999999999999991118, 1.000000000000000000 ) ) ;
#17848 = ORIENTED_EDGE ( 'NONE', *, *, #3079, .T. ) ;
#17849 = ORIENTED_EDGE ( 'NONE', *, *, #6084, .F. ) ;
#17850 = LINE ( 'NONE', #8230, #2731 ) ;
#17851 = VERTEX_POINT ( 'NONE', #7618 ) ;
#17852 = DIRECTION ( 'NONE',  ( -1.000000000000000000, 0.000000000000000000, 0.000000000000000000 ) ) ;
#17853 = EDGE_CURVE ( 'NONE', #17894, #200, #20002, .T. ) ;
#17854 = ORIENTED_EDGE ( 'NONE', *, *, #9045, .T. ) ;
#17855 = CARTESIAN_POINT ( 'NONE',  ( 7.097191417683177406, -22.77556120703057729, 5.229004561291656472 ) ) ;
#17856 = DIRECTION ( 'NONE',  ( 4.625929269271486900E-15, 1.000000000000000000, 0.000000000000000000 ) ) ;
#17857 = CARTESIAN_POINT ( 'NONE',  ( -2.702705060698113115, -10.69015907548275379, 2.777197378435510622 ) ) ;
#17858 = CARTESIAN_POINT ( 'NONE',  ( 2.534747216115884161, -9.671180236796224960, 2.515503256513427210 ) ) ;
#17859 = CARTESIAN_POINT ( 'NONE',  ( -9.152808582316794173, -21.22443879296942626, 5.229004561291660025 ) ) ;
#17860 = ADVANCED_FACE ( 'NONE', ( #19905 ), #12039, .T. ) ;
#17861 = CARTESIAN_POINT ( 'NONE',  ( 11.50344141768317563, -22.05068747287765873, 5.250000000000000888 ) ) ;
#17862 = DIRECTION ( 'NONE',  ( 1.000000000000000000, 0.000000000000000000, -0.000000000000000000 ) ) ;
#17863 = CARTESIAN_POINT ( 'NONE',  ( -5.034691417683178294, -20.22900456129164581, 2.825813738724747726 ) ) ;
#17864 = ORIENTED_EDGE ( 'NONE', *, *, #4167, .T. ) ;
#17865 = CARTESIAN_POINT ( 'NONE',  ( 9.246558582316795949, -21.94931252712234127, 6.000000000000001776 ) ) ;
#17866 = CARTESIAN_POINT ( 'NONE',  ( 12.91308523408712183, -5.701695678577235249, 5.798858176249892082 ) ) ;
#17867 = CARTESIAN_POINT ( 'NONE',  ( -12.62499999999998224, -20.24999999999991829, 4.333333333333343695 ) ) ;
#17868 = ORIENTED_EDGE ( 'NONE', *, *, #4669, .F. ) ;
#17869 = LINE ( 'NONE', #11490, #6946 ) ;
#17870 = CARTESIAN_POINT ( 'NONE',  ( -15.61404127825609223, 4.999999999999999112, 1.000000000000000000 ) ) ;
#17871 = VERTEX_POINT ( 'NONE', #17234 ) ;
#17872 = SURFACE_STYLE_USAGE ( .BOTH. , #9204 ) ;
#17873 = ORIENTED_EDGE ( 'NONE', *, *, #3743, .T. ) ;
#17874 = ADVANCED_FACE ( 'NONE', ( #854 ), #10967, .T. ) ;
#17875 = CARTESIAN_POINT ( 'NONE',  ( 0.000000000000000000, 0.000000000000000000, 1.000000000000000000 ) ) ;
#17876 = VECTOR ( 'NONE', #12982, 1000.000000000000000 ) ;
#17877 = VERTEX_POINT ( 'NONE', #17338 ) ;
#17878 = CARTESIAN_POINT ( 'NONE',  ( -5.590308582316794173, -21.32581373872472597, 1.729004561291657582 ) ) ;
#17879 = CARTESIAN_POINT ( 'NONE',  ( 13.12503131243110843, 5.001581277770153378, 5.166347330538456184 ) ) ;
#17880 = PLANE ( 'NONE',  #19847 ) ;
#17881 = AXIS2_PLACEMENT_3D ( 'NONE', #18686, #17108, #4246 ) ;
#17882 = CARTESIAN_POINT ( 'NONE',  ( 13.15498530132288479, 5.764257716805535559, 4.916666666666649199 ) ) ;
#17883 = CARTESIAN_POINT ( 'NONE',  ( 4.687312169500630787, -21.51559725698340131, 5.182386163300424009 ) ) ;
#17884 = CARTESIAN_POINT ( 'NONE',  ( -13.37597619100657198, -20.20070235416671167, 4.815535977982682070 ) ) ;
#17885 = CARTESIAN_POINT ( 'NONE',  ( 12.24655858231679595, -21.94931252712234127, 6.000000000000001776 ) ) ;
#17886 = CARTESIAN_POINT ( 'NONE',  ( -13.12519991495504712, 4.260095705229160146, 6.739971950528219402 ) ) ;
#17887 = CARTESIAN_POINT ( 'NONE',  ( -5.590308582316795949, -21.01515356694490322, 0.9790045612916562501 ) ) ;
#17888 = CARTESIAN_POINT ( 'NONE',  ( -14.49999999999998579, -19.49999999999999645, 4.000000000000000000 ) ) ;
#17889 = DIRECTION ( 'NONE',  ( 0.000000000000000000, -1.000000000000000000, 0.000000000000000000 ) ) ;
#17890 = VECTOR ( 'NONE', #19339, 1000.000000000000000 ) ;
#17891 = CARTESIAN_POINT ( 'NONE',  ( 12.62155858231679417, -22.99999999999999645, 3.550687472877652073 ) ) ;
#17892 = CARTESIAN_POINT ( 'NONE',  ( -9.065941417683177406, -23.20159541128344927, 2.226721677130534705 ) ) ;
#17893 = VERTEX_POINT ( 'NONE', #4380 ) ;
#17894 = VERTEX_POINT ( 'NONE', #3020 ) ;
#17895 = CARTESIAN_POINT ( 'NONE',  ( 13.84042474920106081, 4.003949834653575124, 5.242612001278796008 ) ) ;
#17896 = DIRECTION ( 'NONE',  ( 1.000000000000000000, -0.000000000000000000, -0.000000000000000000 ) ) ;
#17897 = FILL_AREA_STYLE ('',( #6606 ) ) ;
#17898 = ORIENTED_EDGE ( 'NONE', *, *, #12309, .T. ) ;
#17899 = DIRECTION ( 'NONE',  ( -1.000000000000000000, 0.000000000000000000, 0.000000000000000000 ) ) ;
#17900 = FACE_BOUND ( 'NONE', #14545, .T. ) ;
#17901 = EDGE_CURVE ( 'NONE', #9026, #1111, #20598, .T. ) ;
#17902 = CARTESIAN_POINT ( 'NONE',  ( 13.81626551376501588, 2.033908445126689557, 5.950679699622869911 ) ) ;
#17903 = CARTESIAN_POINT ( 'NONE',  ( 15.06494360078803041, 0.000000000000000000, 1.000000000000000000 ) ) ;
#17904 = CARTESIAN_POINT ( 'NONE',  ( -14.99999999999998224, -17.49999999999999645, 4.000000000000000000 ) ) ;
#17905 = CARTESIAN_POINT ( 'NONE',  ( -9.805650798910056309, 4.999999999999999112, 1.000000000000000000 ) ) ;
#17906 = CARTESIAN_POINT ( 'NONE',  ( -12.62599079447150885, -20.19996487918709249, 4.820256282269618886 ) ) ;
#17907 = CARTESIAN_POINT ( 'NONE',  ( 7.559058582316794173, -20.72672167713054137, 4.701595411283463477 ) ) ;
#17908 = DIRECTION ( 'NONE',  ( -1.000000000000000000, 0.000000000000000000, 0.000000000000000000 ) ) ;
#17909 = CARTESIAN_POINT ( 'NONE',  ( 13.12503131243110843, 5.001581277770153378, 5.166347330538456184 ) ) ;
#17910 = CARTESIAN_POINT ( 'NONE',  ( -1.743623630681728542, -9.116095536440919744, 2.372946416531167557 ) ) ;
#17911 = CARTESIAN_POINT ( 'NONE',  ( -13.84863765609603625, 3.668701632846259830, 5.985835949623216301 ) ) ;
#17912 = DIRECTION ( 'NONE',  ( 1.000000000000000000, 0.000000000000000000, 0.000000000000000000 ) ) ;
#17913 = CARTESIAN_POINT ( 'NONE',  ( 10.19094141768317563, -23.27327832286946219, 4.701595411283453707 ) ) ;
#17914 = CARTESIAN_POINT ( 'NONE',  ( -6.152808582316795949, -21.53509896474924901, 4.479004561291659137 ) ) ;
#17915 = EDGE_LOOP ( 'NONE', ( #12123, #15682, #4133, #18839 ) ) ;
#17916 = CARTESIAN_POINT ( 'NONE',  ( 12.62499999999998224, -20.99999999999998934, 4.166666666666637653 ) ) ;
#17917 = CARTESIAN_POINT ( 'NONE',  ( 13.12529397354238192, 5.014845663890295846, 3.666666666666500873 ) ) ;
#17918 = CARTESIAN_POINT ( 'NONE',  ( -26.04469207716614321, -2.255140518769849223E-14, 0.000000000000000000 ) ) ;
#17919 = VERTEX_POINT ( 'NONE', #9397 ) ;
#17920 = ORIENTED_EDGE ( 'NONE', *, *, #7098, .F. ) ;
#17921 = CARTESIAN_POINT ( 'NONE',  ( 8.119520639128047890, 9.000000000000001776, 1.000000000000000000 ) ) ;
#17922 = EDGE_CURVE ( 'NONE', #14806, #814, #12426, .T. ) ;
#17923 = LINE ( 'NONE', #771, #1569 ) ;
#17924 = DIRECTION ( 'NONE',  ( 0.000000000000000000, 0.1264857625231113059, 0.9919684228235025047 ) ) ;
#17925 = EDGE_CURVE ( 'NONE', #1866, #382, #15179, .T. ) ;
#17926 = CARTESIAN_POINT ( 'NONE',  ( 23.31633994409548549, 0.000000000000000000, 1.000000000000000000 ) ) ;
#17927 = CARTESIAN_POINT ( 'NONE',  ( 2.031432063436913182, -10.08997855658269671, 1.680444048616273722 ) ) ;
#17928 = FACE_OUTER_BOUND ( 'NONE', #12975, .T. ) ;
#17929 = EDGE_CURVE ( 'NONE', #14618, #17122, #11931, .T. ) ;
#17930 = CARTESIAN_POINT ( 'NONE',  ( -11.74178095869206828, 0.000000000000000000, 0.000000000000000000 ) ) ;
#17931 = CARTESIAN_POINT ( 'NONE',  ( 12.73406432005743305, -20.51439999008355741, 3.536278562595261299 ) ) ;
#17932 = DIRECTION ( 'NONE',  ( 0.000000000000000000, -0.000000000000000000, 1.000000000000000000 ) ) ;
#17933 = CARTESIAN_POINT ( 'NONE',  ( -8.684058582316794173, -20.79840458871652942, 2.226721677130544030 ) ) ;
#17934 = CARTESIAN_POINT ( 'NONE',  ( -3.302240162463773832, -9.695145533921818881, 2.714273006325518711 ) ) ;
#17935 = ORIENTED_EDGE ( 'NONE', *, *, #15760, .T. ) ;
#17936 = CARTESIAN_POINT ( 'NONE',  ( -12.63036675113625407, -19.22897906761645004, 4.757923088130392664 ) ) ;
#17937 = EDGE_CURVE ( 'NONE', #6555, #4233, #8144, .T. ) ;
#17938 = CARTESIAN_POINT ( 'NONE',  ( -11.30905858231679417, -23.27327832286945153, 2.298404588716537411 ) ) ;
#17939 = CARTESIAN_POINT ( 'NONE',  ( -8.128441417683175629, -20.24999999999999289, 3.550687472877664952 ) ) ;
#17940 = ORIENTED_EDGE ( 'NONE', *, *, #16276, .T. ) ;
#17941 = CARTESIAN_POINT ( 'NONE',  ( 13.83710853266996388, 3.836480899831821834, 5.239411421715695738 ) ) ;
#17942 =( LENGTH_UNIT ( ) NAMED_UNIT ( * ) SI_UNIT ( .MILLI., .METRE. ) );
#17943 = ORIENTED_EDGE ( 'NONE', *, *, #17411, .F. ) ;
#17944 = VERTEX_POINT ( 'NONE', #3429 ) ;
#17945 = LINE ( 'NONE', #14594, #18761 ) ;
#17946 = ORIENTED_EDGE ( 'NONE', *, *, #12843, .T. ) ;
#17947 = LINE ( 'NONE', #14810, #11105 ) ;
#17948 = EDGE_CURVE ( 'NONE', #431, #734, #14605, .T. ) ;
#17949 = AXIS2_PLACEMENT_3D ( 'NONE', #6795, #7105, #5427 ) ;
#17950 = ORIENTED_EDGE ( 'NONE', *, *, #15654, .T. ) ;
#17951 = CARTESIAN_POINT ( 'NONE',  ( -14.49999999999998579, -25.49999999999999645, 4.000000000000000000 ) ) ;
#17952 = DIRECTION ( 'NONE',  ( 0.000000000000000000, -1.000000000000000000, 0.000000000000000000 ) ) ;
#17953 = CYLINDRICAL_SURFACE ( 'NONE', #4299, 1.499999999999996891 ) ;
#17954 = DIRECTION ( 'NONE',  ( 1.000000000000000000, 0.000000000000000000, -0.000000000000000000 ) ) ;
#17955 = PLANE ( 'NONE',  #3285 ) ;
#17956 = DIRECTION ( 'NONE',  ( 0.000000000000000000, 1.000000000000000000, -0.000000000000000000 ) ) ;
#17957 = CARTESIAN_POINT ( 'NONE',  ( 10.09719141768317741, -22.77556120703057729, 5.229004561291655584 ) ) ;
#17958 = CARTESIAN_POINT ( 'NONE',  ( -8.376396343307449754, 0.000000000000000000, 1.000000000000000000 ) ) ;
#17959 = EDGE_CURVE ( 'NONE', #13259, #11125, #3530, .T. ) ;
#17960 = CARTESIAN_POINT ( 'NONE',  ( -4.753441417683176518, -21.94931252712233061, 1.749999999999998446 ) ) ;
#17961 = ORIENTED_EDGE ( 'NONE', *, *, #2498, .F. ) ;
#17962 = CARTESIAN_POINT ( 'NONE',  ( 11.02780858231679595, -24.47900456129166358, 4.586221378810390270 ) ) ;
#17963 = CARTESIAN_POINT ( 'NONE',  ( 13.10624331898488037, 4.052787608736739600, 6.006964772046813117 ) ) ;
#17964 = CARTESIAN_POINT ( 'NONE',  ( -12.62503117662529739, -20.24842558042254836, 4.565011198945062354 ) ) ;
#17965 = VERTEX_POINT ( 'NONE', #14506 ) ;
#17966 = VECTOR ( 'NONE', #5934, 1000.000000000000000 ) ;
#17967 = DIRECTION ( 'NONE',  ( -0.000000000000000000, -0.000000000000000000, -1.000000000000000000 ) ) ;
#17968 = LINE ( 'NONE', #13055, #3645 ) ;
#17969 = EDGE_LOOP ( 'NONE', ( #5906, #5059, #9941, #14280 ) ) ;
#17970 = MANIFOLD_SOLID_BREP ( 'Mirror1', #13645 ) ;
#17971 = APPLICATION_PROTOCOL_DEFINITION ( 'draft international standard', 'automotive_design', 1998, #12945 ) ;
#17972 = ORIENTED_EDGE ( 'NONE', *, *, #10110, .F. ) ;
#17973 = EDGE_CURVE ( 'NONE', #7153, #13440, #12932, .T. ) ;
#17974 = CARTESIAN_POINT ( 'NONE',  ( 12.76889623635853788, -19.95450346923866647, 3.531415919227487432 ) ) ;
#17975 = EDGE_CURVE ( 'NONE', #20454, #10227, #3220, .T. ) ;
#17976 = EDGE_LOOP ( 'NONE', ( #6678, #5084, #4401, #5105 ) ) ;
#17977 = LINE ( 'NONE', #8468, #9629 ) ;
#17978 = CARTESIAN_POINT ( 'NONE',  ( 13.10821839766814279, 4.152529082241303904, 5.997503362667785609 ) ) ;
#17979 = VECTOR ( 'NONE', #16490, 1000.000000000000000 ) ;
#17980 = LINE ( 'NONE', #8471, #13805 ) ;
#17981 = VECTOR ( 'NONE', #12733, 1000.000000000000000 ) ;
#17982 = CARTESIAN_POINT ( 'NONE',  ( 12.66849571425264287, -18.05346643024382303, 5.533233176248494978 ) ) ;
#17983 = PLANE ( 'NONE',  #9354 ) ;
#17984 = CARTESIAN_POINT ( 'NONE',  ( 10.65280858231679595, -20.91377862118960351, 5.979004561291660913 ) ) ;
#17985 = CARTESIAN_POINT ( 'NONE',  ( -12.62499999999998224, -20.24999999999998934, 4.166666666666636765 ) ) ;
#17986 = EDGE_CURVE ( 'NONE', #20705, #11975, #87, .T. ) ;
#17987 = CARTESIAN_POINT ( 'NONE',  ( -11.12844141768317741, -19.49999999999998934, 3.550687472877664952 ) ) ;
#17988 = CARTESIAN_POINT ( 'NONE',  ( 0.000000000000000000, 9.000000000000001776, 1.000000000000000000 ) ) ;
#17989 = CARTESIAN_POINT ( 'NONE',  ( -18.69064177244175795, 0.000000000000000000, 1.000000000000000000 ) ) ;
#17990 = VECTOR ( 'NONE', #16052, 1000.000000000000000 ) ;
#17991 = CARTESIAN_POINT ( 'NONE',  ( 12.52780858231679773, -22.97900456129165647, 3.964901035250747885 ) ) ;
#17992 = CARTESIAN_POINT ( 'NONE',  ( -4.378441417683176518, -23.74999999999999645, 3.449312527122335492 ) ) ;
#17993 = AXIS2_PLACEMENT_3D ( 'NONE', #8117, #9570, #19312 ) ;
#17994 = EDGE_LOOP ( 'NONE', ( #3923, #787, #7492, #12305 ) ) ;
#17995 = ORIENTED_EDGE ( 'NONE', *, *, #15201, .F. ) ;
#17996 = CARTESIAN_POINT ( 'NONE',  ( 13.84504075139246915, 3.487057945321567765, 5.981929699623240282 ) ) ;
#17997 = AXIS2_PLACEMENT_3D ( 'NONE', #822, #11799, #8668 ) ;
#17998 = LINE ( 'NONE', #8583, #11440 ) ;
#17999 = EDGE_LOOP ( 'NONE', ( #14650, #13874, #8504, #5539 ) ) ;
#18000 = CARTESIAN_POINT ( 'NONE',  ( 14.31494360078803041, 11.64110105645932691, 10.00000000000000000 ) ) ;
#18001 = DIRECTION ( 'NONE',  ( 0.000000000000000000, 1.000000000000000000, 0.000000000000000000 ) ) ;
#18002 = DIRECTION ( 'NONE',  ( 1.000000000000000000, 5.204170427930446527E-15, -0.000000000000000000 ) ) ;
#18003 = CARTESIAN_POINT ( 'NONE',  ( 13.37597619100657198, -20.20070235416671167, 4.815535977982682070 ) ) ;
#18004 = AXIS2_PLACEMENT_3D ( 'NONE', #14286, #17335, #6362 ) ;
#18005 = AXIS2_PLACEMENT_3D ( 'NONE', #13116, #19514, #5165 ) ;
#18006 = LINE ( 'NONE', #3676, #17876 ) ;
#18007 = CARTESIAN_POINT ( 'NONE',  ( 3.365018999794965548, -10.14078633184679923, 2.828722465802024910 ) ) ;
#18008 = AXIS2_PLACEMENT_3D ( 'NONE', #13383, #10467, #11814 ) ;
#18009 = DIRECTION ( 'NONE',  ( 1.000000000000000000, 0.000000000000000000, 0.000000000000000000 ) ) ;
#18010 = CARTESIAN_POINT ( 'NONE',  ( -12.62500000000002132, -19.49999999999450040, 3.833333333368183382 ) ) ;
#18011 = CARTESIAN_POINT ( 'NONE',  ( 9.527808582316794173, -23.72900456129165292, 4.275561207030568411 ) ) ;
#18012 = VECTOR ( 'NONE', #11976, 1000.000000000000000 ) ;
#18013 = DIRECTION ( 'NONE',  ( 0.000000000000000000, 1.000000000000000000, -0.000000000000000000 ) ) ;
#18014 = CARTESIAN_POINT ( 'NONE',  ( 12.68288333306630378, -17.32689168014509207, 5.548858176248425700 ) ) ;
#18015 = EDGE_CURVE ( 'NONE', #12851, #2944, #6474, .T. ) ;
#18016 = CARTESIAN_POINT ( 'NONE',  ( -8.376396343307449754, 0.000000000000000000, 1.000000000000000000 ) ) ;
#18017 = CARTESIAN_POINT ( 'NONE',  ( 11.02780858231679595, -22.97900456129165647, 3.964901035250747885 ) ) ;
#18018 = CARTESIAN_POINT ( 'NONE',  ( 8.784691417683177406, -23.77099543870834353, 4.174186261275252718 ) ) ;
#18019 = CARTESIAN_POINT ( 'NONE',  ( -7.934058582316796837, -22.67126532539354855, 4.242948236979545484 ) ) ;
#18020 = ORIENTED_EDGE ( 'NONE', *, *, #5268, .T. ) ;
#18021 = CARTESIAN_POINT ( 'NONE',  ( 13.90439771357353038, 5.734584535470497180, 4.942866369314573127 ) ) ;
#18022 = CARTESIAN_POINT ( 'NONE',  ( 13.12529397354238192, 5.014845663890295846, 4.583333333333296622 ) ) ;
#18023 = DIRECTION ( 'NONE',  ( -0.000000000000000000, -0.000000000000000000, -1.000000000000000000 ) ) ;
#18024 = EDGE_LOOP ( 'NONE', ( #3822, #2147, #11413, #19937 ) ) ;
#18025 =( REPRESENTATION_RELATIONSHIP ('NONE','NONE', #1880, #6161 ) REPRESENTATION_RELATIONSHIP_WITH_TRANSFORMATION ( #915 )SHAPE_REPRESENTATION_RELATIONSHIP( ) );
#18026 = VECTOR ( 'NONE', #11134, 1000.000000000000000 ) ;
#18027 = ORIENTED_EDGE ( 'NONE', *, *, #11154, .T. ) ;
#18028 = CARTESIAN_POINT ( 'NONE',  ( -14.00000000000000000, 0.000000000000000000, 2.000000000000000000 ) ) ;
#18029 = EDGE_CURVE ( 'NONE', #2724, #13538, #15969, .T. ) ;
#18030 = VECTOR ( 'NONE', #16061, 1000.000000000000000 ) ;
#18031 = FACE_OUTER_BOUND ( 'NONE', #7149, .T. ) ;
#18032 = DIRECTION ( 'NONE',  ( 0.000000000000000000, -1.000000000000000000, 0.000000000000000000 ) ) ;
#18033 = LINE ( 'NONE', #7158, #16348 ) ;
#18034 = CARTESIAN_POINT ( 'NONE',  ( 1.717920576997000737, -9.114924032904250240, 2.372645551019823884 ) ) ;
#18035 = DIRECTION ( 'NONE',  ( 1.000000000000000000, 0.000000000000000000, 0.000000000000000000 ) ) ;
#18036 = AXIS2_PLACEMENT_3D ( 'NONE', #11216, #10138, #1491 ) ;
#18037 = LINE ( 'NONE', #9879, #5718 ) ;
#18038 = CARTESIAN_POINT ( 'NONE',  ( 24.62918902992234038, 10.00000000000000000, 0.000000000000000000 ) ) ;
#18039 = AXIS2_PLACEMENT_3D ( 'NONE', #1793, #16229, #8180 ) ;
#18040 = CARTESIAN_POINT ( 'NONE',  ( -11.00000000000000000, -24.49999999999999289, 4.000000000000000000 ) ) ;
#18041 = CARTESIAN_POINT ( 'NONE',  ( -7.184058582316794173, -20.79840458871652942, 2.226721677130544030 ) ) ;
#18042 = CARTESIAN_POINT ( 'NONE',  ( -2.171407406650392780, -8.432416083433171394, 2.389978857884845986 ) ) ;
#18043 = ORIENTED_EDGE ( 'NONE', *, *, #5779, .T. ) ;
#18044 = MANIFOLD_SOLID_BREP ( 'Boss-Extrude2', #4618 ) ;
#18045 = CARTESIAN_POINT ( 'NONE',  ( -12.62917185724685254, -19.28932120903463598, 4.753410794856941735 ) ) ;
#18046 = CARTESIAN_POINT ( 'NONE',  ( -10.09030858231679595, -21.32581373872472597, 1.729004561291657582 ) ) ;
#18047 = AXIS2_PLACEMENT_3D ( 'NONE', #17621, #15844, #3291 ) ;
#18048 = EDGE_CURVE ( 'NONE', #6863, #7723, #4788, .T. ) ;
#18049 = CARTESIAN_POINT ( 'NONE',  ( -7.097191417683177406, -22.77556120703057729, 5.229004561291655584 ) ) ;
#18050 = ORIENTED_EDGE ( 'NONE', *, *, #1622, .F. ) ;
#18051 = CARTESIAN_POINT ( 'NONE',  ( 13.84495141469777479, 4.232546442235974204, 5.040078719623224401 ) ) ;
#18052 = LINE ( 'NONE', #9993, #5040 ) ;
#18053 = ORIENTED_EDGE ( 'NONE', *, *, #3079, .F. ) ;
#18054 = VERTEX_POINT ( 'NONE', #9498 ) ;
#18055 = LINE ( 'NONE', #3613, #716 ) ;
#18056 = ORIENTED_EDGE ( 'NONE', *, *, #9240, .T. ) ;
#18057 = CARTESIAN_POINT ( 'NONE',  ( 0.000000000000000000, 9.000000000000001776, 1.000000000000000000 ) ) ;
#18058 = ADVANCED_FACE ( 'NONE', ( #19640 ), #702, .T. ) ;
#18059 = ADVANCED_FACE ( 'NONE', ( #13552 ), #15021, .F. ) ;
#18060 = AXIS2_PLACEMENT_3D ( 'NONE', #6790, #2079, #14833 ) ;
#18061 = VERTEX_POINT ( 'NONE', #3736 ) ;
#18062 = AXIS2_PLACEMENT_3D ( 'NONE', #16900, #18586, #13864 ) ;
#18063 = CARTESIAN_POINT ( 'NONE',  ( 4.940941417683177406, -20.72672167713052715, 2.298404588716546293 ) ) ;
#18064 = DIRECTION ( 'NONE',  ( 0.000000000000000000, -0.000000000000000000, 1.000000000000000000 ) ) ;
#18065 = VECTOR ( 'NONE', #19582, 1000.000000000000000 ) ;
#18066 = CARTESIAN_POINT ( 'NONE',  ( 9.555650798910054533, 9.000000000000001776, 0.000000000000000000 ) ) ;
#18067 = CARTESIAN_POINT ( 'NONE',  ( 0.000000000000000000, 9.000000000000001776, 1.000000000000000000 ) ) ;
#18068 = DIRECTION ( 'NONE',  ( -0.000000000000000000, 0.000000000000000000, 1.000000000000000000 ) ) ;
#18069 = CARTESIAN_POINT ( 'NONE',  ( 12.62499999998404299, -20.99999999996810729, 2.793053905886972998 ) ) ;
#18070 = DIRECTION ( 'NONE',  ( 0.000000000000000000, 0.000000000000000000, 1.000000000000000000 ) ) ;
#18071 = CARTESIAN_POINT ( 'NONE',  ( 9.815941417683177406, -20.79840458871654363, 4.773278322869464851 ) ) ;
#18072 = PLANE ( 'NONE',  #855 ) ;
#18073 = CARTESIAN_POINT ( 'NONE',  ( -9.159691417683175629, -22.36352608949543352, 2.479004561291652031 ) ) ;
#18074 = EDGE_CURVE ( 'NONE', #19969, #18591, #18273, .T. ) ;
#18075 = CARTESIAN_POINT ( 'NONE',  ( -7.090308582316795061, -21.01515356694490322, 0.9790045612916562501 ) ) ;
#18076 = EDGE_LOOP ( 'NONE', ( #8639, #9084, #717, #3076 ) ) ;
#18077 = CARTESIAN_POINT ( 'NONE',  ( 13.08094078691552831, 2.775009739235173356, 5.981149842915306714 ) ) ;
#18078 = CARTESIAN_POINT ( 'NONE',  ( -13.13084019862132479, 4.544930030374419339, 6.677052771569639944 ) ) ;
#18079 = VECTOR ( 'NONE', #17789, 1000.000000000000000 ) ;
#18080 = ORIENTED_EDGE ( 'NONE', *, *, #8813, .F. ) ;
#18081 = VECTOR ( 'NONE', #670, 1000.000000000000000 ) ;
#18082 = CARTESIAN_POINT ( 'NONE',  ( 21.17243175760212637, 0.000000000000000000, 1.000000000000000000 ) ) ;
#18083 = DIRECTION ( 'NONE',  ( 1.000000000000000000, 0.000000000000000000, 0.000000000000000000 ) ) ;
#18084 = VECTOR ( 'NONE', #16867, 1000.000000000000000 ) ;
#18085 = EDGE_LOOP ( 'NONE', ( #19944, #11473, #10204, #2243 ) ) ;
#18086 = VECTOR ( 'NONE', #1846, 1000.000000000000227 ) ;
#18087 = ORIENTED_EDGE ( 'NONE', *, *, #1570, .T. ) ;
#18088 = CARTESIAN_POINT ( 'NONE',  ( 13.26617719913702587, -19.98584313357335773, 3.463688470049236745 ) ) ;
#18089 = ORIENTED_EDGE ( 'NONE', *, *, #19002, .F. ) ;
#18090 = EDGE_CURVE ( 'NONE', #9890, #17965, #11781, .T. ) ;
#18091 = PLANE ( 'NONE',  #13986 ) ;
#18092 = CARTESIAN_POINT ( 'NONE',  ( 12.65650603190776025, -18.65894538865861563, 5.520212342915047365 ) ) ;
#18093 = VECTOR ( 'NONE', #1348, 1000.000000000000000 ) ;
#18094 = CARTESIAN_POINT ( 'NONE',  ( 0.000000000000000000, 10.00000000000000000, 1.000000000000000000 ) ) ;
#18095 = DIRECTION ( 'NONE',  ( 1.000000000000000000, 5.204170427930446527E-15, -0.000000000000000000 ) ) ;
#18096 = AXIS2_PLACEMENT_3D ( 'NONE', #12264, #4326, #5999 ) ;
#18097 = CARTESIAN_POINT ( 'NONE',  ( 13.15498530132288479, 5.764257716805535559, 4.666666666666618113 ) ) ;
#18098 = LINE ( 'NONE', #10141, #19387 ) ;
#18099 = CARTESIAN_POINT ( 'NONE',  ( 12.71530858231679417, -24.52099543870834708, 2.515153566944913432 ) ) ;
#18100 = CARTESIAN_POINT ( 'NONE',  ( -12.62499999999998401, -20.24999999999998934, 2.439580858552613751 ) ) ;
#18101 = CARTESIAN_POINT ( 'NONE',  ( -7.378441417683177406, -24.50000000000000000, 3.449312527122335048 ) ) ;
#18102 = EDGE_CURVE ( 'NONE', #12575, #5162, #7087, .T. ) ;
#18103 = EDGE_CURVE ( 'NONE', #10774, #1441, #13650, .T. ) ;
#18104 = CARTESIAN_POINT ( 'NONE',  ( 19.19064177244175440, 11.64110105645932691, 10.00000000000000000 ) ) ;
#18105 = CARTESIAN_POINT ( 'NONE',  ( 8.876396343307449754, 0.000000000000000000, 0.000000000000000000 ) ) ;
#18106 = CARTESIAN_POINT ( 'NONE',  ( 7.090308582316795061, -21.63647391050454871, 2.479004561291657804 ) ) ;
#18107 = DIRECTION ( 'NONE',  ( 0.000000000000000000, 0.8660254037844364872, 0.5000000000000036637 ) ) ;
#18108 = ORIENTED_EDGE ( 'NONE', *, *, #16161, .F. ) ;
#18109 = EDGE_CURVE ( 'NONE', #9991, #10193, #6621, .T. ) ;
#18110 = EDGE_LOOP ( 'NONE', ( #18442, #8323, #11361, #11024 ) ) ;
#18111 = CARTESIAN_POINT ( 'NONE',  ( 13.87470602645761986, 4.985154336109792972, 3.000000000000000000 ) ) ;
#18112 = DIRECTION ( 'NONE',  ( 0.000000000000000000, -0.8660254037844364872, -0.5000000000000036637 ) ) ;
#18113 = EDGE_LOOP ( 'NONE', ( #2155, #7167, #2773, #15143 ) ) ;
#18114 = VECTOR ( 'NONE', #8576, 1000.000000000000000 ) ;
#18115 = LINE ( 'NONE', #13087, #17461 ) ;
#18116 = CARTESIAN_POINT ( 'NONE',  ( -15.00000000000000000, 0.000000000000000000, 1.000000000000000000 ) ) ;
#18117 = ADVANCED_FACE ( 'NONE', ( #11881 ), #16388, .T. ) ;
#18118 = CARTESIAN_POINT ( 'NONE',  ( -3.999999999999999112, -2.500000000000047518, 7.000000000000000000 ) ) ;
#18119 = CARTESIAN_POINT ( 'NONE',  ( 13.85593616229004610, 4.037276195647738319, 5.992122970672676630 ) ) ;
#18120 = DIRECTION ( 'NONE',  ( -1.000000000000000000, -6.938893903907232322E-16, 0.000000000000000000 ) ) ;
#18121 = CARTESIAN_POINT ( 'NONE',  ( 1.513434189748285918, -8.364917468222230923, 2.372643865078341019 ) ) ;
#18122 = DIRECTION ( 'NONE',  ( 0.000000000000000000, 1.000000000000000000, 0.000000000000000000 ) ) ;
#18123 = CARTESIAN_POINT ( 'NONE',  ( -12.62500000000002132, -19.50000000000273559, 4.083333333315724012 ) ) ;
#18124 = CARTESIAN_POINT ( 'NONE',  ( 6.434058582316794173, -23.20159541128345992, 4.773278322869455970 ) ) ;
#18125 = FACE_OUTER_BOUND ( 'NONE', #18085, .T. ) ;
#18126 = CARTESIAN_POINT ( 'NONE',  ( 13.05696142222617695, 1.564051822406025583, 5.955108176248398166 ) ) ;
#18127 = VECTOR ( 'NONE', #4956, 1000.000000000000000 ) ;
#18128 = CARTESIAN_POINT ( 'NONE',  ( -0.2815691515810352930, -9.114917468222230923, 2.372643865078523984 ) ) ;
#18129 = CARTESIAN_POINT ( 'NONE',  ( 10.46530858231679595, -20.97900456129165647, 3.863526089495444626 ) ) ;
#18130 = CARTESIAN_POINT ( 'NONE',  ( 10.56594141768317741, -23.20159541128344927, 2.226721677130534705 ) ) ;
#18131 = CARTESIAN_POINT ( 'NONE',  ( -12.52780858231679595, -23.72900456129165647, 4.275561207030568411 ) ) ;
#18132 = ORIENTED_EDGE ( 'NONE', *, *, #6760, .F. ) ;
#18133 = CARTESIAN_POINT ( 'NONE',  ( 13.12860732321105139, 4.432169822159808703, 6.709107302035562270 ) ) ;
#18134 = CARTESIAN_POINT ( 'NONE',  ( 12.63478567848856571, -19.00582323632600890, 4.762720106674273701 ) ) ;
#18135 = LINE ( 'NONE', #1079, #4005 ) ;
#18136 = ORIENTED_EDGE ( 'NONE', *, *, #858, .F. ) ;
#18137 = ORIENTED_EDGE ( 'NONE', *, *, #14774, .F. ) ;
#18138 = DIRECTION ( 'NONE',  ( 0.000000000000000000, -1.000000000000000000, 0.000000000000000000 ) ) ;
#18139 = EDGE_CURVE ( 'NONE', #14572, #16495, #3935, .T. ) ;
#18140 = DIRECTION ( 'NONE',  ( 0.000000000000000000, -0.000000000000000000, 1.000000000000000000 ) ) ;
#18141 = DIRECTION ( 'NONE',  ( -0.000000000000000000, -0.000000000000000000, -1.000000000000000000 ) ) ;
#18142 = CARTESIAN_POINT ( 'NONE',  ( -26.19203811574920593, 11.64110105645932691, 10.00000000000000000 ) ) ;
#18143 = CARTESIAN_POINT ( 'NONE',  ( 1.700193846275138032, -9.865151716929458914, 2.372704024825938340 ) ) ;
#18144 = DIRECTION ( 'NONE',  ( 0.000000000000000000, -0.000000000000000000, -1.000000000000000000 ) ) ;
#18145 = FACE_OUTER_BOUND ( 'NONE', #599, .T. ) ;
#18146 = CARTESIAN_POINT ( 'NONE',  ( 13.37500000067116268, -20.29298605568190084, 3.448842523571910679 ) ) ;
#18147 = CARTESIAN_POINT ( 'NONE',  ( -2.567175533087980188, -9.771398394011347577, 2.541241281345096859 ) ) ;
#18148 = CARTESIAN_POINT ( 'NONE',  ( -8.590308582316794173, -21.32581373872472597, 1.729004561291657582 ) ) ;
#18149 = CARTESIAN_POINT ( 'NONE',  ( -3.636036383999129207, -10.90885478516162976, 2.275977788322152584 ) ) ;
#18150 = ORIENTED_EDGE ( 'NONE', *, *, #5440, .T. ) ;
#18151 = CARTESIAN_POINT ( 'NONE',  ( -13.37503747255156306, -19.49810763614315690, 4.531249681074674740 ) ) ;
#18152 = CARTESIAN_POINT ( 'NONE',  ( -8.402808582316794173, -22.77556120703056308, 1.770995438708339975 ) ) ;
#18153 = VECTOR ( 'NONE', #4904, 1000.000000000000000 ) ;
#18154 = CARTESIAN_POINT ( 'NONE',  ( -6.722191417683177406, -20.27099543870833998, 4.275561207030583510 ) ) ;
#18155 = ORIENTED_EDGE ( 'NONE', *, *, #18029, .T. ) ;
#18156 = CARTESIAN_POINT ( 'NONE',  ( 13.38921792038197900, -19.53199502070850357, 5.456033026503027017 ) ) ;
#18157 = FACE_OUTER_BOUND ( 'NONE', #18113, .T. ) ;
#18158 = ORIENTED_EDGE ( 'NONE', *, *, #15724, .F. ) ;
#18159 = EDGE_LOOP ( 'NONE', ( #16526, #8538, #11228, #17935 ) ) ;
#18160 = CARTESIAN_POINT ( 'NONE',  ( 0.000000000000000000, 9.000000000000001776, 1.000000000000000000 ) ) ;
#18161 = ORIENTED_EDGE ( 'NONE', *, *, #10636, .T. ) ;
#18162 = DIRECTION ( 'NONE',  ( 0.000000000000000000, 0.000000000000000000, 1.000000000000000000 ) ) ;
#18163 = ORIENTED_EDGE ( 'NONE', *, *, #9871, .F. ) ;
#18164 = DIRECTION ( 'NONE',  ( 0.000000000000000000, 1.000000000000000000, 0.000000000000000000 ) ) ;
#18165 = FACE_OUTER_BOUND ( 'NONE', #688, .T. ) ;
#18166 = EDGE_CURVE ( 'NONE', #3797, #17800, #10322, .T. ) ;
#18167 = LINE ( 'NONE', #13447, #5645 ) ;
#18168 = CARTESIAN_POINT ( 'NONE',  ( 4.066879903460562495, -13.96783368734915776, 3.061584679647603391 ) ) ;
#18169 = CARTESIAN_POINT ( 'NONE',  ( -7.465308582316795061, -20.22900456129164937, 4.174186261275266929 ) ) ;
#18170 = CARTESIAN_POINT ( 'NONE',  ( 13.90439735423812273, 5.734566389025032684, 4.791666666666684726 ) ) ;
#18171 = DIRECTION ( 'NONE',  ( 0.000000000000000000, -0.000000000000000000, 1.000000000000000000 ) ) ;
#18172 = EDGE_CURVE ( 'NONE', #2500, #19250, #902, .T. ) ;
#18173 = EDGE_CURVE ( 'NONE', #5029, #4594, #2162, .T. ) ;
#18174 = CARTESIAN_POINT ( 'NONE',  ( 10.00344141768317741, -22.05068747287766229, 4.499999999999999112 ) ) ;
#18175 = CARTESIAN_POINT ( 'NONE',  ( -12.64387510712649565, -19.29680709011273976, 5.506486987317513737 ) ) ;
#18176 = CARTESIAN_POINT ( 'NONE',  ( -9.347191417683177406, -21.53509896474923835, 2.520995438708346192 ) ) ;
#18177 = CARTESIAN_POINT ( 'NONE',  ( -6.152808582316795949, -20.91377862118960351, 5.979004561291660913 ) ) ;
#18178 = ORIENTED_EDGE ( 'NONE', *, *, #8620, .T. ) ;
#18179 = CARTESIAN_POINT ( 'NONE',  ( 13.10821839766814279, 4.152529082241303904, 5.997503362667785609 ) ) ;
#18180 = CARTESIAN_POINT ( 'NONE',  ( -12.62499999999998401, -20.24999999999998934, 2.439580858552613751 ) ) ;
#18181 = ORIENTED_EDGE ( 'NONE', *, *, #16659, .T. ) ;
#18182 = CARTESIAN_POINT ( 'NONE',  ( 0.000000000000000000, -9.114917468222230923, 2.372643865078340575 ) ) ;
#18183 = DIRECTION ( 'NONE',  ( 0.000000000000000000, 0.000000000000000000, -1.000000000000000000 ) ) ;
#18184 = EDGE_LOOP ( 'NONE', ( #12536, #14899, #17961, #16786 ) ) ;
#18185 = VERTEX_POINT ( 'NONE', #15131 ) ;
#18186 = CARTESIAN_POINT ( 'NONE',  ( 13.06532418593161893, -19.87503328927329704, 3.491089126739379989 ) ) ;
#18187 = ORIENTED_EDGE ( 'NONE', *, *, #8397, .F. ) ;
#18188 = LINE ( 'NONE', #16598, #1637 ) ;
#18189 = CARTESIAN_POINT ( 'NONE',  ( 13.12512971825177033, 5.006550771716304915, 5.133277049491872468 ) ) ;
#18190 = EDGE_CURVE ( 'NONE', #20631, #6657, #14916, .T. ) ;
#18191 = CARTESIAN_POINT ( 'NONE',  ( -0.9854920305337622199, -8.364917468222230923, 1.622643865078341907 ) ) ;
#18192 = DIRECTION ( 'NONE',  ( 1.000000000000000000, 0.000000000000000000, 0.000000000000000000 ) ) ;
#18193 = DIRECTION ( 'NONE',  ( -5.204170427930446527E-15, 1.000000000000000000, 0.000000000000000000 ) ) ;
#18194 =( BOUNDED_SURFACE ( )  B_SPLINE_SURFACE ( 3, 3, ( 
 ( #6670, #10112, #16086, #16487, #2159, #14401, #84, #182, #6472, #17643, #3318, #4884, #8142, #14504, #16284, #6566, #3426, #17858, #4990, #1855, #11369, #17757, #13041, #11478, #1955, #13646, #18581, #899, #5404, #18482, #7396, #8951, #16579, #18269, #8755, #13549, #18380, #17001, #11776, #11878 ),
 ( #8643, #4143, #5608, #15017, #15223, #19950, #11980, #19852, #20159, #8542, #3931, #4043, #8856, #10624, #12090, #20056, #5503, #14913, #698, #15325, #10317, #7084, #1004, #16686, #7284, #13758, #2366, #15126, #589, #5721, #13448, #10526, #16895, #19746, #10428, #6975, #16796, #2565, #802, #5822 ),
 ( #13345, #18168, #7185, #3833, #12189, #2465, #4245, #10212, #2257, #15534, #17107, #11045, #1422, #20259, #9262, #18685, #15841, #9065, #1218, #20573, #15633, #1320, #5919, #7899, #15435, #4352, #10938, #18793, #17207, #12702, #4555, #14261, #3095, #18996, #2990, #7698, #10737, #12400, #1519, #17306 ),
 ( #13858, #2884, #20669, #9470, #2787, #20475, #4459, #6328, #1119, #7496, #10844, #2677, #4653, #19105, #4759, #11144, #9163, #12290, #14066, #17419, #7593, #13959, #12596, #20363, #18896, #6026, #6131, #12500, #9366, #6225, #15741, #7804, #14166, #11239, #5167, #19413, #8214, #14577, #13118, #468 ),
 ( #6750, #17617, #12807, #2032, #19516, #17730, #8422, #3288, #3398, #8309, #19205, #14790, #13212, #17831, #11548, #9670, #12902, #17927, #6442, #6843, #3596, #15939, #13012, #9566, #19611, #9777, #3498, #364, #9976, #14479, #3194, #16056, #16357, #5072, #250, #6641, #5266, #17512, #158, #1619 ),
 ( #4858, #8000, #14370, #16164, #57, #1729, #1827, #14684, #8113, #6541, #19307, #9876, #4962, #11341, #11449, #16259, #1926, #7365, #13728, #20133, #774, #20027, #666, #15096, #4012, #19825, #16461, #18143, #2135, #8516, #7159, #16769, #977, #10398, #14886, #875, #10499, #12063, #19715, #7055 ),
 ( #563, #13314, #10186, #10286, #6942, #16868, #11751, #7258, #8726, #3808, #18349, #2335, #16656, #2231, #2538, #11645, #13420, #13523, #11952, #8927, #5375, #5479, #16556, #2439, #3907, #4117, #11852, #8616, #18034, #3704, #19925, #8831, #15198, #15297, #5581, #10087, #14988, #18244, #13620, #5689 ) ),
 .UNSPECIFIED., .T., .F., .F. ) 
 B_SPLINE_SURFACE_WITH_KNOTS ( ( 4, 3, 4 ),
 ( 4, 2, 2, 2, 2, 2, 2, 2, 2, 2, 2, 2, 2, 2, 2, 2, 2, 2, 2, 4 ),
 ( 0.000000000000000000, 0.5000000000000000000, 1.000000000000000000 ),
 ( 0.000000000000000000, 0.3100443560520446118, 0.4650665340780669177, 0.5425776230910780429, 0.5813331675975836887, 0.6007109398508364562, 0.6200887121040892236, 0.6309950902025724950, 0.6419014683010558775, 0.6637142244980225314, 0.7073397368919559502, 0.7509652492858893691, 0.7727780054828560230, 0.7836843835813394055, 0.7945907616798226769, 0.8074288390748337596, 0.8202669164698448423, 0.8459430712598670077, 0.8972953808399113385, 1.000000000000000000 ),
 .UNSPECIFIED. ) 
 GEOMETRIC_REPRESENTATION_ITEM ( )  RATIONAL_B_SPLINE_SURFACE ( (
 ( 1.000000000000000000, 1.000000000000000000, 1.000000000000000000, 1.000000000000000000, 1.000000000000000000, 1.000000000000000000, 1.000000000000000000, 1.000000000000000000, 1.000000000000000000, 1.000000000000000000, 1.000000000000000000, 1.000000000000000000, 1.000000000000000000, 1.000000000000000000, 1.000000000000000000, 1.000000000000000000, 1.000000000000000000, 1.000000000000000000, 1.000000000000000000, 1.000000000000000000, 1.000000000000000000, 1.000000000000000000, 1.000000000000000000, 1.000000000000000000, 1.000000000000000000, 1.000000000000000000, 1.000000000000000000, 1.000000000000000000, 1.000000000000000000, 1.000000000000000000, 1.000000000000000000, 1.000000000000000000, 1.000000000000000000, 1.000000000000000000, 1.000000000000000000, 1.000000000000000000, 1.000000000000000000, 1.000000000000000000, 1.000000000000000000, 1.000000000000000000),
 ( 0.3333333333333333703, 0.3333333333333333703, 0.3333333333333333703, 0.3333333333333333703, 0.3333333333333333703, 0.3333333333333333703, 0.3333333333333333703, 0.3333333333333333703, 0.3333333333333333703, 0.3333333333333333703, 0.3333333333333333703, 0.3333333333333333703, 0.3333333333333333703, 0.3333333333333333703, 0.3333333333333333703, 0.3333333333333333703, 0.3333333333333333703, 0.3333333333333333703, 0.3333333333333333703, 0.3333333333333333703, 0.3333333333333333703, 0.3333333333333333703, 0.3333333333333333703, 0.3333333333333333703, 0.3333333333333333703, 0.3333333333333333703, 0.3333333333333333703, 0.3333333333333333703, 0.3333333333333333703, 0.3333333333333333703, 0.3333333333333333703, 0.3333333333333333703, 0.3333333333333333703, 0.3333333333333333703, 0.3333333333333333703, 0.3333333333333333703, 0.3333333333333333703, 0.3333333333333333703, 0.3333333333333333703, 0.3333333333333333703),
 ( 0.3333333333333333703, 0.3333333333333333703, 0.3333333333333333703, 0.3333333333333333703, 0.3333333333333333703, 0.3333333333333333703, 0.3333333333333333703, 0.3333333333333333703, 0.3333333333333333703, 0.3333333333333333703, 0.3333333333333333703, 0.3333333333333333703, 0.3333333333333333703, 0.3333333333333333703, 0.3333333333333333703, 0.3333333333333333703, 0.3333333333333333703, 0.3333333333333333703, 0.3333333333333333703, 0.3333333333333333703, 0.3333333333333333703, 0.3333333333333333703, 0.3333333333333333703, 0.3333333333333333703, 0.3333333333333333703, 0.3333333333333333703, 0.3333333333333333703, 0.3333333333333333703, 0.3333333333333333703, 0.3333333333333333703, 0.3333333333333333703, 0.3333333333333333703, 0.3333333333333333703, 0.3333333333333333703, 0.3333333333333333703, 0.3333333333333333703, 0.3333333333333333703, 0.3333333333333333703, 0.3333333333333333703, 0.3333333333333333703),
 ( 1.000000000000000000, 1.000000000000000000, 1.000000000000000000, 1.000000000000000000, 1.000000000000000000, 1.000000000000000000, 1.000000000000000000, 1.000000000000000000, 1.000000000000000000, 1.000000000000000000, 1.000000000000000000, 1.000000000000000000, 1.000000000000000000, 1.000000000000000000, 1.000000000000000000, 1.000000000000000000, 1.000000000000000000, 1.000000000000000000, 1.000000000000000000, 1.000000000000000000, 1.000000000000000000, 1.000000000000000000, 1.000000000000000000, 1.000000000000000000, 1.000000000000000000, 1.000000000000000000, 1.000000000000000000, 1.000000000000000000, 1.000000000000000000, 1.000000000000000000, 1.000000000000000000, 1.000000000000000000, 1.000000000000000000, 1.000000000000000000, 1.000000000000000000, 1.000000000000000000, 1.000000000000000000, 1.000000000000000000, 1.000000000000000000, 1.000000000000000000),
 ( 0.3333333333333333703, 0.3333333333333333703, 0.3333333333333333703, 0.3333333333333333703, 0.3333333333333333703, 0.3333333333333333703, 0.3333333333333333703, 0.3333333333333333703, 0.3333333333333333703, 0.3333333333333333703, 0.3333333333333333703, 0.3333333333333333703, 0.3333333333333333703, 0.3333333333333333703, 0.3333333333333333703, 0.3333333333333333703, 0.3333333333333333703, 0.3333333333333333703, 0.3333333333333333703, 0.3333333333333333703, 0.3333333333333333703, 0.3333333333333333703, 0.3333333333333333703, 0.3333333333333333703, 0.3333333333333333703, 0.3333333333333333703, 0.3333333333333333703, 0.3333333333333333703, 0.3333333333333333703, 0.3333333333333333703, 0.3333333333333333703, 0.3333333333333333703, 0.3333333333333333703, 0.3333333333333333703, 0.3333333333333333703, 0.3333333333333333703, 0.3333333333333333703, 0.3333333333333333703, 0.3333333333333333703, 0.3333333333333333703),
 ( 0.3333333333333333703, 0.3333333333333333703, 0.3333333333333333703, 0.3333333333333333703, 0.3333333333333333703, 0.3333333333333333703, 0.3333333333333333703, 0.3333333333333333703, 0.3333333333333333703, 0.3333333333333333703, 0.3333333333333333703, 0.3333333333333333703, 0.3333333333333333703, 0.3333333333333333703, 0.3333333333333333703, 0.3333333333333333703, 0.3333333333333333703, 0.3333333333333333703, 0.3333333333333333703, 0.3333333333333333703, 0.3333333333333333703, 0.3333333333333333703, 0.3333333333333333703, 0.3333333333333333703, 0.3333333333333333703, 0.3333333333333333703, 0.3333333333333333703, 0.3333333333333333703, 0.3333333333333333703, 0.3333333333333333703, 0.3333333333333333703, 0.3333333333333333703, 0.3333333333333333703, 0.3333333333333333703, 0.3333333333333333703, 0.3333333333333333703, 0.3333333333333333703, 0.3333333333333333703, 0.3333333333333333703, 0.3333333333333333703),
 ( 1.000000000000000000, 1.000000000000000000, 1.000000000000000000, 1.000000000000000000, 1.000000000000000000, 1.000000000000000000, 1.000000000000000000, 1.000000000000000000, 1.000000000000000000, 1.000000000000000000, 1.000000000000000000, 1.000000000000000000, 1.000000000000000000, 1.000000000000000000, 1.000000000000000000, 1.000000000000000000, 1.000000000000000000, 1.000000000000000000, 1.000000000000000000, 1.000000000000000000, 1.000000000000000000, 1.000000000000000000, 1.000000000000000000, 1.000000000000000000, 1.000000000000000000, 1.000000000000000000, 1.000000000000000000, 1.000000000000000000, 1.000000000000000000, 1.000000000000000000, 1.000000000000000000, 1.000000000000000000, 1.000000000000000000, 1.000000000000000000, 1.000000000000000000, 1.000000000000000000, 1.000000000000000000, 1.000000000000000000, 1.000000000000000000, 1.000000000000000000) ) ) 
 REPRESENTATION_ITEM ( '' )  SURFACE ( )  );
#18195 = CARTESIAN_POINT ( 'NONE',  ( 13.12529397354238192, 5.014845663890295846, 4.583333333333296622 ) ) ;
#18196 = CARTESIAN_POINT ( 'NONE',  ( 0.000000000000000000, 4.999999999999999112, 1.000000000000000000 ) ) ;
#18197 = EDGE_CURVE ( 'NONE', #4996, #4809, #2943, .T. ) ;
#18198 = EDGE_CURVE ( 'NONE', #2900, #6116, #8451, .T. ) ;
#18199 = CARTESIAN_POINT ( 'NONE',  ( 6.434058582316796837, -23.73192549717337130, 5.303608408759367343 ) ) ;
#18200 = CARTESIAN_POINT ( 'NONE',  ( -13.10985494974158705, 3.485174961951963191, 6.746454579156001330 ) ) ;
#18201 = CARTESIAN_POINT ( 'NONE',  ( -9.440941417683177406, -20.19639159124061933, 1.768074502826635586 ) ) ;
#18202 = ORIENTED_EDGE ( 'NONE', *, *, #7276, .T. ) ;
#18203 = PLANE ( 'NONE',  #10055 ) ;
#18204 = CARTESIAN_POINT ( 'NONE',  ( 13.49999999999998401, -25.49999999999999645, 4.000000000000000000 ) ) ;
#18205 = EDGE_CURVE ( 'NONE', #2799, #14875, #10431, .T. ) ;
#18206 = CARTESIAN_POINT ( 'NONE',  ( 12.34030858231679773, -22.36352608949544418, 4.520995438708343528 ) ) ;
#18207 = LINE ( 'NONE', #10247, #14322 ) ;
#18208 = EDGE_LOOP ( 'NONE', ( #11111, #13131, #8533, #5000 ) ) ;
#18209 = ORIENTED_EDGE ( 'NONE', *, *, #16437, .F. ) ;
#18210 = CARTESIAN_POINT ( 'NONE',  ( 13.40382044110196347, -18.79456772435387890, 5.502763032956559108 ) ) ;
#18211 = DIRECTION ( 'NONE',  ( -0.000000000000000000, -0.000000000000000000, -1.000000000000000000 ) ) ;
#18212 = ORIENTED_EDGE ( 'NONE', *, *, #13507, .F. ) ;
#18213 = CARTESIAN_POINT ( 'NONE',  ( -4.999999999999998224, -7.500000000000047073, 9.999999999999998224 ) ) ;
#18214 = DIRECTION ( 'NONE',  ( 0.000000000000000000, -0.000000000000000000, 1.000000000000000000 ) ) ;
#18215 = CARTESIAN_POINT ( 'NONE',  ( 0.000000000000000000, 4.999999999999999112, 1.000000000000000000 ) ) ;
#18216 = CARTESIAN_POINT ( 'NONE',  ( 13.39542766346049518, -19.21840299524461315, 5.493648449623241170 ) ) ;
#18217 = EDGE_CURVE ( 'NONE', #20635, #14903, #16800, .T. ) ;
#18218 = DIRECTION ( 'NONE',  ( -0.000000000000000000, -0.000000000000000000, -1.000000000000000000 ) ) ;
#18219 = CARTESIAN_POINT ( 'NONE',  ( 4.066879903460562495, -13.96783368734915776, 3.061584679647603391 ) ) ;
#18220 = FACE_OUTER_BOUND ( 'NONE', #11281, .T. ) ;
#18221 = VECTOR ( 'NONE', #15838, 1000.000000000000000 ) ;
#18222 = CARTESIAN_POINT ( 'NONE',  ( -13.12512971825177033, 5.006550771716304915, 5.133277049491872468 ) ) ;
#18223 = LINE ( 'NONE', #10167, #7770 ) ;
#18224 = LINE ( 'NONE', #6922, #7734 ) ;
#18225 = CARTESIAN_POINT ( 'NONE',  ( 12.69247507894198712, -16.84250851341299082, 5.559274842915185033 ) ) ;
#18226 = FACE_OUTER_BOUND ( 'NONE', #17218, .T. ) ;
#18227 = CARTESIAN_POINT ( 'NONE',  ( 12.43405858231679595, -22.67126532539354855, 4.242948236979545484 ) ) ;
#18228 = EDGE_CURVE ( 'NONE', #2639, #12514, #20061, .T. ) ;
#18229 = CARTESIAN_POINT ( 'NONE',  ( 9.722191417683177406, -20.27099543870833998, 4.275561207030583510 ) ) ;
#18230 = CARTESIAN_POINT ( 'NONE',  ( -10.65280858231679240, -21.22443879296942626, 5.229004561291659137 ) ) ;
#18231 = VERTEX_POINT ( 'NONE', #14169 ) ;
#18232 = CARTESIAN_POINT ( 'NONE',  ( 12.65017171054692113, -19.72882861737994631, 6.192581331858542981 ) ) ;
#18233 = CARTESIAN_POINT ( 'NONE',  ( 12.62499999999998224, -19.49999999999998934, 4.291666666666699825 ) ) ;
#18234 = DIRECTION ( 'NONE',  ( 2.312964634635730039E-15, -1.000000000000000000, 0.000000000000000000 ) ) ;
#18235 = VERTEX_POINT ( 'NONE', #1009 ) ;
#18236 = PRODUCT_DEFINITION_CONTEXT ( 'detailed design', #19780, 'design' ) ;
#18237 = ORIENTED_EDGE ( 'NONE', *, *, #6489, .F. ) ;
#18238 = DIRECTION ( 'NONE',  ( -0.000000000000000000, -0.000000000000000000, -1.000000000000000000 ) ) ;
#18239 = LINE ( 'NONE', #19822, #10256 ) ;
#18240 = ADVANCED_FACE ( 'NONE', ( #17210 ), #13962, .T. ) ;
#18241 = EDGE_CURVE ( 'NONE', #12822, #14996, #14070, .T. ) ;
#18242 = PLANE ( 'NONE',  #14655 ) ;
#18243 = CARTESIAN_POINT ( 'NONE',  ( 6.183390479346035917, 0.000000000000000000, 1.000000000000000000 ) ) ;
#18244 = CARTESIAN_POINT ( 'NONE',  ( 0.5631383031621635116, -9.114917468222230923, 2.372643865078341019 ) ) ;
#18245 = DIRECTION ( 'NONE',  ( 0.000000000000000000, -1.000000000000000000, 0.000000000000000000 ) ) ;
#18246 = LINE ( 'NONE', #13214, #10401 ) ;
#18247 = CARTESIAN_POINT ( 'NONE',  ( 13.20683383907801733, -20.56345410174260735, 3.472004214064662975 ) ) ;
#18248 = CARTESIAN_POINT ( 'NONE',  ( -2.559937518207947793, -9.746075135043517079, 2.534737762559237773 ) ) ;
#18249 = CARTESIAN_POINT ( 'NONE',  ( -9.527808582316792396, -23.72900456129165647, 4.275561207030568411 ) ) ;
#18250 = CARTESIAN_POINT ( 'NONE',  ( -3.537356407578672535, -11.36437789272258669, 3.142965222332344766 ) ) ;
#18251 = EDGE_LOOP ( 'NONE', ( #8462, #17099, #2672, #4367 ) ) ;
#18252 = AXIS2_PLACEMENT_3D ( 'NONE', #6323, #12801, #12696 ) ;
#18253 = CARTESIAN_POINT ( 'NONE',  ( -13.57153706873194032, -9.574878029060977624, 4.950999963380944280 ) ) ;
#18254 = CARTESIAN_POINT ( 'NONE',  ( -5.027808582316793284, -23.72900456129165647, 4.275561207030568411 ) ) ;
#18255 = ADVANCED_FACE ( 'NONE', ( #7596 ), #7807, .T. ) ;
#18256 = CARTESIAN_POINT ( 'NONE',  ( -9.253441417683177406, -21.94931252712233061, 2.499999999999999112 ) ) ;
#18257 = ORIENTED_EDGE ( 'NONE', *, *, #15201, .T. ) ;
#18258 = CARTESIAN_POINT ( 'NONE',  ( 13.41820805991576826, -18.06799297425606454, 5.518388032956592859 ) ) ;
#18259 = PLANE ( 'NONE',  #8047 ) ;
#18260 = ORIENTED_EDGE ( 'NONE', *, *, #20136, .F. ) ;
#18261 = ORIENTED_EDGE ( 'NONE', *, *, #1314, .F. ) ;
#18262 = CARTESIAN_POINT ( 'NONE',  ( 15.50000000000000178, -20.99999999999999645, 4.000000000000000000 ) ) ;
#18263 = ORIENTED_EDGE ( 'NONE', *, *, #18576, .F. ) ;
#18264 = CARTESIAN_POINT ( 'NONE',  ( -13.38238173943565990, -19.87722215849730034, 5.285856107751903288 ) ) ;
#18265 = EDGE_LOOP ( 'NONE', ( #8741, #17174, #5786, #17825 ) ) ;
#18266 = CARTESIAN_POINT ( 'NONE',  ( 5.034691417683179182, -20.22900456129164581, 2.825813738724748170 ) ) ;
#18267 = CARTESIAN_POINT ( 'NONE',  ( 19.19064177244175440, 10.00000000000000000, 1.000000000000000000 ) ) ;
#18268 = CARTESIAN_POINT ( 'NONE',  ( 11.49178095869207006, 9.000000000000001776, 0.000000000000000000 ) ) ;
#18269 = CARTESIAN_POINT ( 'NONE',  ( 1.407845757905374695, -9.114917468222230923, 2.372643865078341019 ) ) ;
#18270 = LINE ( 'NONE', #10113, #19661 ) ;
#18271 = AXIS2_PLACEMENT_3D ( 'NONE', #12190, #2566, #9263 ) ;
#18272 = CARTESIAN_POINT ( 'NONE',  ( 12.64802275499843454, -19.83735087257960927, 6.157588447769994922 ) ) ;
#18273 = LINE ( 'NONE', #8758, #5963 ) ;
#18274 = CARTESIAN_POINT ( 'NONE',  ( 9.253441417683177406, -21.94931252712233061, 2.499999999999999112 ) ) ;
#18275 = FACE_OUTER_BOUND ( 'NONE', #15954, .T. ) ;
#18276 = CARTESIAN_POINT ( 'NONE',  ( -4.003441417683175629, -22.05068747287766229, 4.499999999999999112 ) ) ;
#18277 = CARTESIAN_POINT ( 'NONE',  ( -8.972191417683177406, -24.47900456129165292, 2.413778621189595963 ) ) ;
#18278 = VERTEX_POINT ( 'NONE', #10627 ) ;
#18279 = CARTESIAN_POINT ( 'NONE',  ( 12.62917185724685254, -19.28932120903463598, 4.753410794856941735 ) ) ;
#18280 = CARTESIAN_POINT ( 'NONE',  ( -13.12503131243110843, 5.001581277770153378, 5.166347330538456184 ) ) ;
#18281 = VERTEX_POINT ( 'NONE', #4146 ) ;
#18282 = VECTOR ( 'NONE', #2730, 1000.000000000000000 ) ;
#18283 = EDGE_CURVE ( 'NONE', #487, #16176, #2681, .T. ) ;
#18284 = CARTESIAN_POINT ( 'NONE',  ( -4.000000000000000000, -8.500000000000000000, 1.000000000000000000 ) ) ;
#18285 = LINE ( 'NONE', #713, #11335 ) ;
#18286 = EDGE_LOOP ( 'NONE', ( #11859, #527, #17011, #12694 ) ) ;
#18287 = ORIENTED_EDGE ( 'NONE', *, *, #2847, .T. ) ;
#18288 = ORIENTED_EDGE ( 'NONE', *, *, #3250, .F. ) ;
#18289 = DIRECTION ( 'NONE',  ( 1.000000000000000000, 0.000000000000000000, 0.000000000000000000 ) ) ;
#18290 = CARTESIAN_POINT ( 'NONE',  ( -7.869520639128047002, 4.999999999999999112, 0.000000000000000000 ) ) ;
#18291 = CARTESIAN_POINT ( 'NONE',  ( -2.830107938415192148, -10.43856789473369950, 1.962583737180462418 ) ) ;
#18292 = DIRECTION ( 'NONE',  ( 1.000000000000000000, 0.000000000000000000, -0.000000000000000000 ) ) ;
#18293 = CARTESIAN_POINT ( 'NONE',  ( -30.80549002841696193, 5.431839045955507927, 1.000000000000000000 ) ) ;
#18294 = CARTESIAN_POINT ( 'NONE',  ( 13.09293046926041626, 3.380488697651010011, 5.994170676248444352 ) ) ;
#18295 = CYLINDRICAL_SURFACE ( 'NONE', #3337, 0.3750000000000003331 ) ;
#18296 = CARTESIAN_POINT ( 'NONE',  ( 5.871558582316795949, -19.49999999999998934, 3.449312527122348371 ) ) ;
#18297 = CARTESIAN_POINT ( 'NONE',  ( -12.72125031657057015, -15.38935901321805133, 5.590524842915047365 ) ) ;
#18298 = CARTESIAN_POINT ( 'NONE',  ( -9.815941417683177406, -20.26807450282663225, 5.303608408759377113 ) ) ;
#18299 = ORIENTED_EDGE ( 'NONE', *, *, #7387, .F. ) ;
#18300 = CARTESIAN_POINT ( 'NONE',  ( 12.15280858231679595, -21.22443879296942626, 5.229004561291659137 ) ) ;
#18301 = FACE_OUTER_BOUND ( 'NONE', #15392, .T. ) ;
#18302 = CARTESIAN_POINT ( 'NONE',  ( -13.86316420010827777, 3.652292105464413297, 6.735515685864076119 ) ) ;
#18303 = EDGE_CURVE ( 'NONE', #17894, #2477, #4356, .T. ) ;
#18304 = CARTESIAN_POINT ( 'NONE',  ( 5.496558582316795949, -22.05068747287764452, 2.499999999999999112 ) ) ;
#18305 = CARTESIAN_POINT ( 'NONE',  ( 10.00000000000000355, -34.99999999999999289, 1.000000000000000000 ) ) ;
#18306 = EDGE_LOOP ( 'NONE', ( #10878, #7223, #12936, #17020 ) ) ;
#18307 = VERTEX_POINT ( 'NONE', #7400 ) ;
#18308 = CARTESIAN_POINT ( 'NONE',  ( 13.87470586348985258, 4.985146106231644225, 5.033049509202228933 ) ) ;
#18309 = DIRECTION ( 'NONE',  ( -0.000000000000000000, -0.000000000000000000, -1.000000000000000000 ) ) ;
#18310 = SURFACE_SIDE_STYLE ('',( #5654 ) ) ;
#18311 = ORIENTED_EDGE ( 'NONE', *, *, #14452, .T. ) ;
#18312 = AXIS2_PLACEMENT_3D ( 'NONE', #4463, #18485, #1221 ) ;
#18313 = DIRECTION ( 'NONE',  ( 5.204170427930446527E-15, -1.000000000000000000, 0.000000000000000000 ) ) ;
#18314 = EDGE_CURVE ( 'NONE', #483, #20175, #4288, .T. ) ;
#18315 = ADVANCED_FACE ( 'NONE', ( #10848 ), #10740, .T. ) ;
#18316 = DIRECTION ( 'NONE',  ( -0.000000000000000000, -0.000000000000000000, -1.000000000000000000 ) ) ;
#18317 = VECTOR ( 'NONE', #2693, 1000.000000000000000 ) ;
#18318 = CARTESIAN_POINT ( 'NONE',  ( 13.12499999999999467, 5.000000000000047073, 3.999999999999996447 ) ) ;
#18319 = CARTESIAN_POINT ( 'NONE',  ( 13.40382044110196347, -18.79456772435387890, 5.502763032956559108 ) ) ;
#18320 =( BOUNDED_CURVE ( )  B_SPLINE_CURVE ( 3, ( #14368, #15631, #11141, #12594 ),
 .UNSPECIFIED., .F., .T. ) 
 B_SPLINE_CURVE_WITH_KNOTS ( ( 4, 4 ),
 ( 0.000000000000000000, 1.468430546537837468E-05 ),
 .UNSPECIFIED. ) 
 CURVE ( )  GEOMETRIC_REPRESENTATION_ITEM ( )  RATIONAL_B_SPLINE_CURVE ( ( 1.000000000000000000, 0.9870550161812301493, 0.9743613912715626268, 0.9619191252709974327 ) ) 
 REPRESENTATION_ITEM ( '' )  );
#18321 = PLANE ( 'NONE',  #5183 ) ;
#18322 = CARTESIAN_POINT ( 'NONE',  ( 0.5631383031621635116, -9.114917468222230923, 2.372643865078341019 ) ) ;
#18323 = CARTESIAN_POINT ( 'NONE',  ( 1.811130159782011528, 0.000000000000000000, 1.000000000000000000 ) ) ;
#18324 = CARTESIAN_POINT ( 'NONE',  ( -12.64917329730235096, -18.27924848622803466, 4.778345106674467324 ) ) ;
#18325 = CARTESIAN_POINT ( 'NONE',  ( 13.87500000000000178, 5.000000000000047962, 4.000000000000000000 ) ) ;
#18326 = FACE_OUTER_BOUND ( 'NONE', #17035, .T. ) ;
#18327 = CARTESIAN_POINT ( 'NONE',  ( -13.85956729540471066, 3.470648417939721231, 6.731609435864099211 ) ) ;
#18328 = VECTOR ( 'NONE', #17309, 1000.000000000000000 ) ;
#18329 = CARTESIAN_POINT ( 'NONE',  ( 0.6250000000000005551, 10.00000000000000000, 1.000000000000000000 ) ) ;
#18330 = CARTESIAN_POINT ( 'NONE',  ( 12.62155858231679417, -22.99999999999999645, 3.550687472877652073 ) ) ;
#18331 = VECTOR ( 'NONE', #16087, 1000.000000000000000 ) ;
#18332 = EDGE_CURVE ( 'NONE', #14809, #382, #13862, .T. ) ;
#18333 = CARTESIAN_POINT ( 'NONE',  ( 6.253441417683176518, -21.94931252712233061, 1.749999999999998446 ) ) ;
#18334 = CARTESIAN_POINT ( 'NONE',  ( -4.717959273841179524, -21.82295283170803302, 4.493595146365858994 ) ) ;
#18335 = EDGE_LOOP ( 'NONE', ( #7434, #1641, #2822, #13977 ) ) ;
#18336 = CARTESIAN_POINT ( 'NONE',  ( 13.14123030749026277, 5.069630528265579805, 6.418963484850015000 ) ) ;
#18337 = CARTESIAN_POINT ( 'NONE',  ( 12.65396917024039958, -18.03705690286155772, 4.783553440007634272 ) ) ;
#18338 = DIRECTION ( 'NONE',  ( 0.000000000000000000, -1.000000000000000000, 0.000000000000000000 ) ) ;
#18339 = VERTEX_POINT ( 'NONE', #17110 ) ;
#18340 = ORIENTED_EDGE ( 'NONE', *, *, #16252, .F. ) ;
#18341 = CARTESIAN_POINT ( 'NONE',  ( 9.000000000000000000, -9.999999999999991118, 2.000000000000000000 ) ) ;
#18342 = VECTOR ( 'NONE', #14682, 1000.000000000000000 ) ;
#18343 = DIRECTION ( 'NONE',  ( -0.000000000000000000, 0.000000000000000000, 1.000000000000000000 ) ) ;
#18344 = VECTOR ( 'NONE', #18521, 1000.000000000000000 ) ;
#18345 = VECTOR ( 'NONE', #4374, 1000.000000000000000 ) ;
#18346 = DIRECTION ( 'NONE',  ( -0.000000000000000000, -0.000000000000000000, -1.000000000000000000 ) ) ;
#18347 = EDGE_CURVE ( 'NONE', #3417, #13354, #18584, .T. ) ;
#18348 = PLANE ( 'NONE',  #19363 ) ;
#18349 = CARTESIAN_POINT ( 'NONE',  ( 2.616536356806028696, -10.07836329504444706, 2.620076000170431296 ) ) ;
#18350 = DIRECTION ( 'NONE',  ( 1.000000000000000000, 0.000000000000000000, 0.000000000000000000 ) ) ;
#18351 = FACE_OUTER_BOUND ( 'NONE', #16042, .T. ) ;
#18352 = CARTESIAN_POINT ( 'NONE',  ( 27.50000000000000355, 3.000000000000000888, 0.000000000000000000 ) ) ;
#18353 = CARTESIAN_POINT ( 'NONE',  ( -6.340308582316793284, -22.67418626127525982, 5.270995438708342640 ) ) ;
#18354 = AXIS2_PLACEMENT_3D ( 'NONE', #9804, #9903, #392 ) ;
#18355 = CARTESIAN_POINT ( 'NONE',  ( -1.948765222931501784, -9.143197003266354983, 1.629906614618163552 ) ) ;
#18356 = VECTOR ( 'NONE', #15404, 1000.000000000000227 ) ;
#18357 = ORIENTED_EDGE ( 'NONE', *, *, #15235, .F. ) ;
#18358 = CARTESIAN_POINT ( 'NONE',  ( -13.09560264576187905, 4.265433610975056133, 4.791666666666684726 ) ) ;
#18359 = CARTESIAN_POINT ( 'NONE',  ( -6.996558582316793284, -22.05068747287764452, 1.749999999999998446 ) ) ;
#18360 = EDGE_CURVE ( 'NONE', #5953, #5929, #7500, .T. ) ;
#18361 = CARTESIAN_POINT ( 'NONE',  ( 12.43405858231679595, -23.73192549717337130, 5.303608408759367343 ) ) ;
#18362 = CARTESIAN_POINT ( 'NONE',  ( -11.87844141768317741, -22.99999999999999645, 3.449312527122335048 ) ) ;
#18363 = AXIS2_PLACEMENT_3D ( 'NONE', #2404, #19888, #525 ) ;
#18364 = ORIENTED_EDGE ( 'NONE', *, *, #14828, .F. ) ;
#18365 = EDGE_CURVE ( 'NONE', #13057, #15932, #20263, .T. ) ;
#18366 = CARTESIAN_POINT ( 'NONE',  ( 13.85528666703740619, 4.004476685417483139, 5.993048563355776182 ) ) ;
#18367 = CARTESIAN_POINT ( 'NONE',  ( -22.81633994409548549, 0.000000000000000000, 1.000000000000000000 ) ) ;
#18368 = ORIENTED_EDGE ( 'NONE', *, *, #11213, .T. ) ;
#18369 = VERTEX_POINT ( 'NONE', #12192 ) ;
#18370 = LINE ( 'NONE', #10615, #8148 ) ;
#18371 = ADVANCED_FACE ( 'NONE', ( #20478 ), #8954, .F. ) ;
#18372 = VERTEX_POINT ( 'NONE', #2994 ) ;
#18373 = CARTESIAN_POINT ( 'NONE',  ( -27.00000000000000000, 0.000000000000000000, 0.000000000000000000 ) ) ;
#18374 = ORIENTED_EDGE ( 'NONE', *, *, #1806, .F. ) ;
#18375 = CARTESIAN_POINT ( 'NONE',  ( 23.60856191738414012, 4.999999999999999112, 1.000000000000000000 ) ) ;
#18376 = EDGE_CURVE ( 'NONE', #3058, #17557, #9166, .T. ) ;
#18377 = FACE_OUTER_BOUND ( 'NONE', #13769, .T. ) ;
#18378 = CIRCLE ( 'NONE', #19383, 0.3749999999999997224 ) ;
#18379 = CARTESIAN_POINT ( 'NONE',  ( 11.00000000000000000, -20.16506350946107418, 5.000000000000000000 ) ) ;
#18380 = CARTESIAN_POINT ( 'NONE',  ( 0.9854920305337621089, -9.114917468222230923, 2.372643865078341019 ) ) ;
#18381 = CARTESIAN_POINT ( 'NONE',  ( 0.000000000000000000, 0.000000000000000000, 4.000000000000000000 ) ) ;
#18382 = VECTOR ( 'NONE', #63, 1000.000000000000000 ) ;
#18383 = AXIS2_PLACEMENT_3D ( 'NONE', #8369, #11398, #5434 ) ;
#18384 = CARTESIAN_POINT ( 'NONE',  ( 12.62505438222622622, -20.99725369757571869, 4.613400783263607252 ) ) ;
#18385 = DIRECTION ( 'NONE',  ( -0.000000000000000000, -0.000000000000000000, -1.000000000000000000 ) ) ;
#18386 = CARTESIAN_POINT ( 'NONE',  ( 3.944195004867016241, -21.61378581760806838, 5.207602947182413899 ) ) ;
#18387 = CARTESIAN_POINT ( 'NONE',  ( -12.62499999999998579, -20.24999999999999289, 3.666666666666653640 ) ) ;
#18388 = CARTESIAN_POINT ( 'NONE',  ( -8.034691417683175629, -20.97900456129164581, 3.136473910504570917 ) ) ;
#18389 = CARTESIAN_POINT ( 'NONE',  ( -11.31594141768317741, -20.26807450282663225, 5.303608408759377113 ) ) ;
#18390 = ORIENTED_EDGE ( 'NONE', *, *, #10873, .F. ) ;
#18391 = CARTESIAN_POINT ( 'NONE',  ( 13.12529397354238192, 5.014845663890295846, 4.583333333333296622 ) ) ;
#18392 = CARTESIAN_POINT ( 'NONE',  ( -13.12529397354238192, 5.014845663890295846, 4.791666666666685614 ) ) ;
#18393 = ORIENTED_EDGE ( 'NONE', *, *, #14183, .F. ) ;
#18394 = LINE ( 'NONE', #15030, #7621 ) ;
#18395 = CARTESIAN_POINT ( 'NONE',  ( -9.000000000000000000, -9.999999999999992895, 1.000000000000000000 ) ) ;
#18396 = VERTEX_POINT ( 'NONE', #18900 ) ;
#18397 = ORIENTED_EDGE ( 'NONE', *, *, #14379, .T. ) ;
#18398 = AXIS2_PLACEMENT_3D ( 'NONE', #19614, #9536, #7964 ) ;
#18399 = VERTEX_POINT ( 'NONE', #10942 ) ;
#18400 = DIRECTION ( 'NONE',  ( -0.000000000000000000, -0.000000000000000000, -1.000000000000000000 ) ) ;
#18401 = EDGE_CURVE ( 'NONE', #17464, #16697, #9370, .T. ) ;
#18402 = DIRECTION ( 'NONE',  ( 0.000000000000000000, -1.000000000000000000, 0.000000000000000000 ) ) ;
#18403 = CARTESIAN_POINT ( 'NONE',  ( -2.780192134145684779, -10.08406280675441735, 1.871539748636713130 ) ) ;
#18404 = DIRECTION ( 'NONE',  ( 1.000000000000000000, 0.000000000000000000, -0.000000000000000000 ) ) ;
#18405 = DIRECTION ( 'NONE',  ( -0.9848077530122080203, 0.1736481776669309696, 0.000000000000000000 ) ) ;
#18406 = PLANE ( 'NONE',  #8011 ) ;
#18407 = CARTESIAN_POINT ( 'NONE',  ( 12.53469141768317741, -19.47900456129164581, 2.515153566944927199 ) ) ;
#18408 = CARTESIAN_POINT ( 'NONE',  ( -13.10372118337080849, 3.925419760224517329, 6.005889426248455010 ) ) ;
#18409 = CARTESIAN_POINT ( 'NONE',  ( -8.784691417683177406, -24.52099543870834708, 4.484846433055073689 ) ) ;
#18410 = AXIS2_PLACEMENT_3D ( 'NONE', #13839, #20242, #14046 ) ;
#18411 = CIRCLE ( 'NONE', #8064, 0.3749999999999998890 ) ;
#18412 = ORIENTED_EDGE ( 'NONE', *, *, #10626, .F. ) ;
#18413 = CARTESIAN_POINT ( 'NONE',  ( 13.27780858231679595, -20.27099543870833642, 2.724438792969431589 ) ) ;
#18414 = CARTESIAN_POINT ( 'NONE',  ( 17.80017143803810242, 9.000000000000001776, 1.000000000000000000 ) ) ;
#18415 = CARTESIAN_POINT ( 'NONE',  ( -13.40653076352726103, -19.40769644187082932, 6.236886054669082746 ) ) ;
#18416 = CARTESIAN_POINT ( 'NONE',  ( 12.71530858231679240, -23.77099543870833998, 2.825813738724734847 ) ) ;
#18417 = CARTESIAN_POINT ( 'NONE',  ( -2.499999999999998668, -19.50000000000000000, 1.000000000000000000 ) ) ;
#18418 = VERTEX_POINT ( 'NONE', #9067 ) ;
#18419 = ORIENTED_EDGE ( 'NONE', *, *, #15555, .F. ) ;
#18420 = CARTESIAN_POINT ( 'NONE',  ( 13.39662663169496781, -19.15785509940297615, 5.494950532956567102 ) ) ;
#18421 = CARTESIAN_POINT ( 'NONE',  ( 2.687849085826861995, 10.00000000000000000, 1.000000000000000000 ) ) ;
#18422 = EDGE_LOOP ( 'NONE', ( #12418, #9505, #2524, #14700, #10920, #11660, #12446, #14223 ) ) ;
#18423 = DIRECTION ( 'NONE',  ( 0.000000000000000000, -1.000000000000000000, 0.000000000000000000 ) ) ;
#18424 = FACE_OUTER_BOUND ( 'NONE', #9512, .T. ) ;
#18425 = CARTESIAN_POINT ( 'NONE',  ( 0.000000000000000000, 10.00000000000000000, 1.000000000000000000 ) ) ;
#18426 = VECTOR ( 'NONE', #13194, 1000.000000000000000 ) ;
#18427 = CARTESIAN_POINT ( 'NONE',  ( 13.87444723674697755, 4.972085455720938185, 5.163895512850782410 ) ) ;
#18428 = DIRECTION ( 'NONE',  ( 1.000000000000000000, 0.000000000000000000, -0.000000000000000000 ) ) ;
#18429 = CARTESIAN_POINT ( 'NONE',  ( 1.126276606324276619, -9.114917468222230923, 2.372643865078341019 ) ) ;
#18430 = EDGE_CURVE ( 'NONE', #3612, #4521, #15439, .T. ) ;
#18431 = LINE ( 'NONE', #18533, #11725 ) ;
#18432 = CARTESIAN_POINT ( 'NONE',  ( -12.63478567848856571, -19.00582323632600890, 4.762720106674273701 ) ) ;
#18433 = CARTESIAN_POINT ( 'NONE',  ( 0.000000000000000000, 9.000000000000001776, 1.000000000000000000 ) ) ;
#18434 = CARTESIAN_POINT ( 'NONE',  ( -18.69064177244175795, 16.00000000000000000, 1.000000000000000000 ) ) ;
#18435 = CARTESIAN_POINT ( 'NONE',  ( -13.41475008041063433, -18.99262093926051520, 6.248536519197435801 ) ) ;
#18436 = CARTESIAN_POINT ( 'NONE',  ( 14.31494360078803041, 10.00000000000000000, 0.000000000000000000 ) ) ;
#18437 = CARTESIAN_POINT ( 'NONE',  ( 10.84030858231679240, -22.67418626127525982, 5.270995438708342640 ) ) ;
#18438 = ADVANCED_FACE ( 'NONE', ( #8005 ), #6645, .F. ) ;
#18439 = AXIS2_PLACEMENT_3D ( 'NONE', #10237, #16603, #2283 ) ;
#18440 = CARTESIAN_POINT ( 'NONE',  ( 5.878441417683177406, -23.74999999999999645, 3.449312527122335492 ) ) ;
#18441 = CARTESIAN_POINT ( 'NONE',  ( -11.02780858231679595, -23.72900456129165647, 4.275561207030568411 ) ) ;
#18442 = ORIENTED_EDGE ( 'NONE', *, *, #2707, .F. ) ;
#18443 = CARTESIAN_POINT ( 'NONE',  ( 12.64183575740756993, -20.14979425091403087, 6.022201559249563907 ) ) ;
#18444 = VECTOR ( 'NONE', #13136, 1000.000000000000000 ) ;
#18445 = CARTESIAN_POINT ( 'NONE',  ( 12.89855869007488209, -5.685286151195387383, 5.049178440009032265 ) ) ;
#18446 = PLANE ( 'NONE',  #19706 ) ;
#18447 = ORIENTED_EDGE ( 'NONE', *, *, #10640, .T. ) ;
#18448 = ORIENTED_EDGE ( 'NONE', *, *, #5819, .F. ) ;
#18449 = DIRECTION ( 'NONE',  ( 0.000000000000000000, 1.000000000000000000, 0.000000000000000000 ) ) ;
#18450 = CARTESIAN_POINT ( 'NONE',  ( -12.63249216759192350, -19.87164553660301536, 5.297612231341934041 ) ) ;
#18451 = CARTESIAN_POINT ( 'NONE',  ( -3.277163086644854229, -14.76879761173520578, 3.824673233536266537 ) ) ;
#18452 = VECTOR ( 'NONE', #253, 1000.000000000000000 ) ;
#18453 = EDGE_CURVE ( 'NONE', #19940, #19480, #3292, .T. ) ;
#18454 = CARTESIAN_POINT ( 'NONE',  ( 30.80549002841696904, 5.431839045955454637, 1.000000000000000000 ) ) ;
#18455 = CARTESIAN_POINT ( 'NONE',  ( -12.62672070884157804, -20.24999999999991473, 3.550922209436377042 ) ) ;
#18456 = LINE ( 'NONE', #7670, #8364 ) ;
#18457 = FACE_OUTER_BOUND ( 'NONE', #149, .T. ) ;
#18458 = CARTESIAN_POINT ( 'NONE',  ( 4.413027396565882832, -21.45855829990031438, 5.554906804930435982 ) ) ;
#18459 = CARTESIAN_POINT ( 'NONE',  ( -10.84030858231679595, -22.98484643305508612, 6.020995438708344416 ) ) ;
#18460 = CARTESIAN_POINT ( 'NONE',  ( -1.407845757905374695, -9.114917468222230923, 1.622643865078341463 ) ) ;
#18461 = VERTEX_POINT ( 'NONE', #4657 ) ;
#18462 = CARTESIAN_POINT ( 'NONE',  ( -13.79214722387705905, 1.565934805775630601, 5.190583296715636230 ) ) ;
#18463 = AXIS2_PLACEMENT_3D ( 'NONE', #4451, #19273, #4926 ) ;
#18464 = DIRECTION ( 'NONE',  ( -0.000000000000000000, -0.000000000000000000, -1.000000000000000000 ) ) ;
#18465 = CARTESIAN_POINT ( 'NONE',  ( 11.59719141768317741, -23.08622137881040359, 5.979004561291654696 ) ) ;
#18466 = CARTESIAN_POINT ( 'NONE',  ( -9.909691417683175629, -21.63647391050456648, 4.520995438708348857 ) ) ;
#18467 = ORIENTED_EDGE ( 'NONE', *, *, #20226, .F. ) ;
#18468 = CARTESIAN_POINT ( 'NONE',  ( 13.37500000000002132, -20.24999999999450040, 3.833333333368183382 ) ) ;
#18469 = LINE ( 'NONE', #10612, #15047 ) ;
#18470 = ORIENTED_EDGE ( 'NONE', *, *, #14477, .F. ) ;
#18471 = ORIENTED_EDGE ( 'NONE', *, *, #4749, .F. ) ;
#18472 = VECTOR ( 'NONE', #7661, 1000.000000000000000 ) ;
#18473 = DIRECTION ( 'NONE',  ( 0.000000000000000000, -1.000000000000000000, 0.000000000000000000 ) ) ;
#18474 = ORIENTED_EDGE ( 'NONE', *, *, #2619, .T. ) ;
#18475 = CARTESIAN_POINT ( 'NONE',  ( -13.39902456816392906, -19.03675930772010361, 5.497554699623231400 ) ) ;
#18476 = EDGE_LOOP ( 'NONE', ( #18808, #692, #2873, #7710, #15037, #14494 ) ) ;
#18477 = CARTESIAN_POINT ( 'NONE',  ( 14.99999999999999645, 3.000000000000003553, 2.000000000000000000 ) ) ;
#18478 = DIRECTION ( 'NONE',  ( 0.000000000000000000, -1.000000000000000000, 0.000000000000000000 ) ) ;
#18479 = EDGE_CURVE ( 'NONE', #6038, #6263, #6545, .T. ) ;
#18480 = ADVANCED_FACE ( 'NONE', ( #12908 ), #11049, .T. ) ;
#18481 = DIRECTION ( 'NONE',  ( 1.000000000000000000, 0.000000000000000000, 0.000000000000000000 ) ) ;
#18482 = CARTESIAN_POINT ( 'NONE',  ( 1.655860418491166941, -9.114909740826840689, 2.372641880528837621 ) ) ;
#18483 = PLANE ( 'NONE',  #17881 ) ;
#18484 = CARTESIAN_POINT ( 'NONE',  ( 13.90439735423812273, 5.734566389025032684, 4.666666666666618113 ) ) ;
#18485 = DIRECTION ( 'NONE',  ( 0.000000000000000000, 1.000000000000000000, 0.000000000000000000 ) ) ;
#18486 = DIRECTION ( 'NONE',  ( 1.000000000000000000, 0.000000000000000000, -0.000000000000000000 ) ) ;
#18487 = FACE_OUTER_BOUND ( 'NONE', #17976, .T. ) ;
#18488 = CARTESIAN_POINT ( 'NONE',  ( 9.815941417683177406, -21.32873467460645145, 4.242948236979555254 ) ) ;
#18489 = CARTESIAN_POINT ( 'NONE',  ( -12.62745083560477966, -20.12623280195927933, 5.001038150054709419 ) ) ;
#18490 = CARTESIAN_POINT ( 'NONE',  ( -7.378441417683177406, -22.99999999999999645, 3.449312527122335048 ) ) ;
#18491 = CARTESIAN_POINT ( 'NONE',  ( -5.121558582316795061, -24.50000000000000000, 3.550687472877651629 ) ) ;
#18492 = ORIENTED_EDGE ( 'NONE', *, *, #8949, .T. ) ;
#18493 = CARTESIAN_POINT ( 'NONE',  ( 12.78345773956433895, -11.49788415197707181, 4.924178440007425550 ) ) ;
#18494 = CARTESIAN_POINT ( 'NONE',  ( -12.72125031657057015, -15.38935901321805133, 5.590524842915047365 ) ) ;
#18495 = ORIENTED_EDGE ( 'NONE', *, *, #12776, .T. ) ;
#18496 = AXIS2_PLACEMENT_3D ( 'NONE', #10673, #843, #17045 ) ;
#18497 = EDGE_CURVE ( 'NONE', #16676, #5259, #8314, .T. ) ;
#18498 = DIRECTION ( 'NONE',  ( -0.000000000000000000, 0.000000000000000000, -1.000000000000000000 ) ) ;
#18499 = DIRECTION ( 'NONE',  ( 0.000000000000000000, 1.000000000000000000, 0.000000000000000000 ) ) ;
#18500 = ORIENTED_EDGE ( 'NONE', *, *, #7303, .F. ) ;
#18501 = PRODUCT_CONTEXT ( 'NONE', #131, 'mechanical' ) ;
#18502 = VERTEX_POINT ( 'NONE', #20576 ) ;
#18503 = ORIENTED_EDGE ( 'NONE', *, *, #669, .F. ) ;
#18504 = DIRECTION ( 'NONE',  ( 0.000000000000000000, -0.000000000000000000, 1.000000000000000000 ) ) ;
#18505 = CARTESIAN_POINT ( 'NONE',  ( 0.000000000000000000, 10.00000000000000000, 1.000000000000000000 ) ) ;
#18506 = EDGE_CURVE ( 'NONE', #19457, #18649, #1734, .T. ) ;
#18507 = ADVANCED_FACE ( 'NONE', ( #14484 ), #19000, .F. ) ;
#18508 = CARTESIAN_POINT ( 'NONE',  ( -1.407845757905374695, -9.114917468222230923, 1.622643865078341463 ) ) ;
#18509 = DIRECTION ( 'NONE',  ( 0.000000000000000000, 0.000000000000000000, 1.000000000000000000 ) ) ;
#18510 = DIRECTION ( 'NONE',  ( 1.000000000000000000, 0.000000000000000000, 0.000000000000000000 ) ) ;
#18511 = DIRECTION ( 'NONE',  ( 1.000000000000000000, 0.000000000000000000, 0.000000000000000000 ) ) ;
#18512 = CARTESIAN_POINT ( 'NONE',  ( 4.934058582316795061, -23.73192549717337130, 5.303608408759367343 ) ) ;
#18513 = CARTESIAN_POINT ( 'NONE',  ( -12.65650603190776025, -18.65894538865861563, 5.520212342915047365 ) ) ;
#18514 = CARTESIAN_POINT ( 'NONE',  ( -6.065941417683177406, -23.73192549717336064, 1.696391591240623331 ) ) ;
#18515 = ORIENTED_EDGE ( 'NONE', *, *, #972, .T. ) ;
#18516 = CARTESIAN_POINT ( 'NONE',  ( 11.96530858231679595, -20.22900456129164937, 4.174186261275266929 ) ) ;
#18517 = DIRECTION ( 'NONE',  ( -1.000000000000000000, -0.000000000000000000, -0.000000000000000000 ) ) ;
#18518 = CARTESIAN_POINT ( 'NONE',  ( -13.41475008041063433, -18.99262093926051520, 6.248536519197435801 ) ) ;
#18519 = EDGE_CURVE ( 'NONE', #7330, #9049, #61, .T. ) ;
#18520 = CARTESIAN_POINT ( 'NONE',  ( 6.527808582316795949, -22.97900456129165647, 3.964901035250747885 ) ) ;
#18521 = DIRECTION ( 'NONE',  ( -0.000000000000000000, -0.000000000000000000, -1.000000000000000000 ) ) ;
#18522 = ORIENTED_EDGE ( 'NONE', *, *, #10983, .F. ) ;
#18523 = EDGE_LOOP ( 'NONE', ( #18393, #3162, #2457, #5400 ) ) ;
#18524 = CARTESIAN_POINT ( 'NONE',  ( 13.37500000000002132, -21.00000000000274269, 4.083333333315724012 ) ) ;
#18525 = LINE ( 'NONE', #2609, #7228 ) ;
#18526 = EDGE_LOOP ( 'NONE', ( #9710, #13924, #19946, #12465 ) ) ;
#18527 = FACE_OUTER_BOUND ( 'NONE', #6384, .T. ) ;
#18528 = ORIENTED_EDGE ( 'NONE', *, *, #19410, .T. ) ;
#18529 = CARTESIAN_POINT ( 'NONE',  ( -9.059058582316794173, -20.72672167713054137, 4.701595411283463477 ) ) ;
#18530 = CARTESIAN_POINT ( 'NONE',  ( 13.87454419214980739, 4.976981703567351367, 5.131312659523921127 ) ) ;
#18531 = DIRECTION ( 'NONE',  ( -0.000000000000000000, -1.000000000000000000, 0.000000000000000000 ) ) ;
#18532 = CARTESIAN_POINT ( 'NONE',  ( 2.722060606927515725, -8.660968749821154944, 1.698675748411476283 ) ) ;
#18533 = CARTESIAN_POINT ( 'NONE',  ( 25.04469207716615031, 4.999999999999999112, 1.000000000000000000 ) ) ;
#18534 = CARTESIAN_POINT ( 'NONE',  ( -13.09123688038123490, 4.044962459253448550, 5.255034774807352704 ) ) ;
#18535 = CARTESIAN_POINT ( 'NONE',  ( 13.18405858231679417, -20.79840458871652942, 2.226721677130544030 ) ) ;
#18536 = CARTESIAN_POINT ( 'NONE',  ( -13.87005939078915873, 4.000499234880882327, 6.742989431566016378 ) ) ;
#18537 = DIRECTION ( 'NONE',  ( 1.000000000000000000, 0.000000000000000000, 0.000000000000000000 ) ) ;
#18538 = CARTESIAN_POINT ( 'NONE',  ( 11.87155858231679417, -20.24999999999999289, 3.449312527122348371 ) ) ;
#18539 = AXIS2_PLACEMENT_3D ( 'NONE', #1673, #16307, #9515 ) ;
#18540 = CARTESIAN_POINT ( 'NONE',  ( 5.503441417683176518, -22.05068747287765873, 5.250000000000000888 ) ) ;
#18541 = CARTESIAN_POINT ( 'NONE',  ( -8.871558582316794173, -20.24999999999999289, 3.449312527122348371 ) ) ;
#18542 = ORIENTED_EDGE ( 'NONE', *, *, #20314, .T. ) ;
#18543 = CARTESIAN_POINT ( 'NONE',  ( 12.78345773956433895, -11.49788415197707181, 4.924178440007425550 ) ) ;
#18544 = CARTESIAN_POINT ( 'NONE',  ( 12.00000000000000178, -26.50000000000000355, 4.000000000000000000 ) ) ;
#18545 = ORIENTED_EDGE ( 'NONE', *, *, #17724, .T. ) ;
#18546 = ORIENTED_EDGE ( 'NONE', *, *, #13595, .T. ) ;
#18547 = DIRECTION ( 'NONE',  ( 1.000000000000000000, -3.469446951953611033E-15, 0.000000000000000000 ) ) ;
#18548 = CARTESIAN_POINT ( 'NONE',  ( -12.62500016093973620, -20.24999187254239175, 4.532396751752561848 ) ) ;
#18549 = CIRCLE ( 'NONE', #7254, 0.4999999999999987232 ) ;
#18550 = CYLINDRICAL_SURFACE ( 'NONE', #19349, 1.499999999999999556 ) ;
#18551 = CARTESIAN_POINT ( 'NONE',  ( -13.38450946332969771, -19.76977210184853462, 5.359796180098093998 ) ) ;
#18552 = CARTESIAN_POINT ( 'NONE',  ( -2.187849085826861550, 0.000000000000000000, 0.000000000000000000 ) ) ;
#18553 = CARTESIAN_POINT ( 'NONE',  ( -12.62499999999998579, -20.24999999999999289, 3.146526952850934755 ) ) ;
#18554 = DIRECTION ( 'NONE',  ( 0.000000000000000000, 0.000000000000000000, -1.000000000000000000 ) ) ;
#18555 = CARTESIAN_POINT ( 'NONE',  ( 0.000000000000000000, 9.000000000000001776, 1.000000000000000000 ) ) ;
#18556 = CARTESIAN_POINT ( 'NONE',  ( -1.619022621591187150, -9.114917468222230923, 2.372643865078341019 ) ) ;
#18557 = CARTESIAN_POINT ( 'NONE',  ( -8.402808582316797725, -23.08622137881038938, 1.020995438708339309 ) ) ;
#18558 = CARTESIAN_POINT ( 'NONE',  ( -1.126276606324276619, -8.364917468222230923, 1.622643865078341907 ) ) ;
#18559 = ORIENTED_EDGE ( 'NONE', *, *, #1187, .F. ) ;
#18560 = CARTESIAN_POINT ( 'NONE',  ( -13.09560264576187905, 4.265433610975056133, 4.833333333333343695 ) ) ;
#18561 = CARTESIAN_POINT ( 'NONE',  ( -13.17791111847408025, 0.000000000000000000, 1.000000000000000000 ) ) ;
#18562 = CARTESIAN_POINT ( 'NONE',  ( 11.12844141768317741, -19.49999999999998934, 3.550687472877664952 ) ) ;
#18563 = CARTESIAN_POINT ( 'NONE',  ( -8.128441417683177406, -20.99999999999999645, 3.550687472877664952 ) ) ;
#18564 = ORIENTED_EDGE ( 'NONE', *, *, #6673, .F. ) ;
#18565 = CARTESIAN_POINT ( 'NONE',  ( 13.84501469867711698, 4.235742283194553259, 2.999999999999999556 ) ) ;
#18566 = DIRECTION ( 'NONE',  ( 1.000000000000000000, 0.000000000000000000, 0.000000000000000000 ) ) ;
#18567 = ORIENTED_EDGE ( 'NONE', *, *, #16928, .F. ) ;
#18568 = VECTOR ( 'NONE', #19238, 1000.000000000000000 ) ;
#18569 = ORIENTED_EDGE ( 'NONE', *, *, #1949, .T. ) ;
#18570 = DIRECTION ( 'NONE',  ( 0.000000000000000000, 0.000000000000000000, 1.000000000000000000 ) ) ;
#18571 = EDGE_CURVE ( 'NONE', #14753, #11489, #256, .T. ) ;
#18572 = ORIENTED_EDGE ( 'NONE', *, *, #13755, .T. ) ;
#18573 = CARTESIAN_POINT ( 'NONE',  ( -13.87470602645761986, 4.985154336109792972, 4.916666666666650087 ) ) ;
#18574 = CARTESIAN_POINT ( 'NONE',  ( -13.67767524182159100, -0.4755849646238735073, 1.001433380786713068 ) ) ;
#18575 = ADVANCED_FACE ( 'NONE', ( #9475 ), #14581, .T. ) ;
#18576 = EDGE_CURVE ( 'NONE', #1583, #18591, #9782, .T. ) ;
#18577 = EDGE_LOOP ( 'NONE', ( #5709, #16184, #13750, #11206 ) ) ;
#18578 = DIRECTION ( 'NONE',  ( -1.734723475976807094E-15, 1.000000000000000000, 0.000000000000000000 ) ) ;
#18579 = CARTESIAN_POINT ( 'NONE',  ( 23.60856191738414012, 0.000000000000000000, 1.000000000000000000 ) ) ;
#18580 = LINE ( 'NONE', #5821, #2641 ) ;
#18581 = CARTESIAN_POINT ( 'NONE',  ( 1.797604806073912709, -9.120796646272857799, 2.374153755450133740 ) ) ;
#18582 = CARTESIAN_POINT ( 'NONE',  ( -15.49999999999999822, -22.99999999999999289, 1.000000000000000000 ) ) ;
#18583 = CARTESIAN_POINT ( 'NONE',  ( 13.11704875914858270, 3.848462337001107070, 6.754267079155989784 ) ) ;
#18584 = LINE ( 'NONE', #10529, #270 ) ;
#18585 = DIRECTION ( 'NONE',  ( -1.000000000000000000, 0.000000000000000000, 0.000000000000000000 ) ) ;
#18586 = DIRECTION ( 'NONE',  ( 1.000000000000000000, 0.000000000000000000, -0.000000000000000000 ) ) ;
#18587 = CARTESIAN_POINT ( 'NONE',  ( 11.50344141768317741, -22.05068747287766229, 4.499999999999999112 ) ) ;
#18588 = CARTESIAN_POINT ( 'NONE',  ( -12.62500000000001954, -20.25000000000274269, 4.083333333315724012 ) ) ;
#18589 = CARTESIAN_POINT ( 'NONE',  ( -8.777808582316797725, -21.02099543870833998, 3.035098964749253003 ) ) ;
#18590 = CARTESIAN_POINT ( 'NONE',  ( -8.315941417683177406, -20.26807450282663225, 5.303608408759377113 ) ) ;
#18591 = VERTEX_POINT ( 'NONE', #16169 ) ;
#18592 = CARTESIAN_POINT ( 'NONE',  ( 13.12270769621861355, 4.884238659038159902, 5.513847264053151065 ) ) ;
#18593 = CARTESIAN_POINT ( 'NONE',  ( -13.06655316810189227, 2.048434989138931961, 5.965524842914772030 ) ) ;
#18594 = EDGE_LOOP ( 'NONE', ( #18982, #4540, #4890, #686 ) ) ;
#18595 = DIRECTION ( 'NONE',  ( -0.000000000000000000, -0.000000000000000000, -1.000000000000000000 ) ) ;
#18596 = EDGE_CURVE ( 'NONE', #1231, #14809, #19209, .T. ) ;
#18597 = FACE_OUTER_BOUND ( 'NONE', #13162, .T. ) ;
#18598 = VERTEX_POINT ( 'NONE', #6229 ) ;
#18599 = CARTESIAN_POINT ( 'NONE',  ( 1.126276606324276619, -9.864917468222230923, 2.372643865078341019 ) ) ;
#18600 = ORIENTED_EDGE ( 'NONE', *, *, #7773, .T. ) ;
#18601 = VERTEX_POINT ( 'NONE', #4863 ) ;
#18602 = DIRECTION ( 'NONE',  ( 1.000000000000000000, 0.000000000000000000, 0.000000000000000000 ) ) ;
#18603 = CARTESIAN_POINT ( 'NONE',  ( -3.499999999999997780, -24.49999999999999289, 1.000000000000000000 ) ) ;
#18604 = CARTESIAN_POINT ( 'NONE',  ( -2.557403344953185442, -14.91030650174552896, 3.668400560659690779 ) ) ;
#18605 = CARTESIAN_POINT ( 'NONE',  ( -2.187849085826861550, 11.64110105645932691, 0.000000000000000000 ) ) ;
#18606 = CARTESIAN_POINT ( 'NONE',  ( 3.999999999999999112, -2.500000000000047518, 7.000000000000000000 ) ) ;
#18607 = EDGE_CURVE ( 'NONE', #19894, #3922, #9881, .T. ) ;
#18608 = CARTESIAN_POINT ( 'NONE',  ( 14.50000000000000000, -20.99999999999998934, 1.000000000000000000 ) ) ;
#18609 = AXIS2_PLACEMENT_3D ( 'NONE', #872, #2228, #10181 ) ;
#18610 = CARTESIAN_POINT ( 'NONE',  ( 7.090308582316795061, -21.01515356694490322, 0.9790045612916562501 ) ) ;
#18611 = CARTESIAN_POINT ( 'NONE',  ( -13.12529380813666435, 5.014837310896125722, 5.033295791462342628 ) ) ;
#18612 = CARTESIAN_POINT ( 'NONE',  ( -9.253441417683177406, -21.94931252712233061, 1.749999999999998446 ) ) ;
#18613 = B_SPLINE_CURVE_WITH_KNOTS ( 'NONE', 3,
 ( #2781, #15527, #18574, #1417, #14161, #20568, #6220, #5912, #15036, #2670 ),
 .UNSPECIFIED., .F., .F.,
 ( 4, 2, 2, 2, 4 ),
 ( 0.000000000000000000, 0.0002648908096818753050, 0.0005297816193637506100, 0.0007946724290456259150, 0.001059563238727501437 ),
 .UNSPECIFIED. ) ;
#18614 = VERTEX_POINT ( 'NONE', #19419 ) ;
#18615 = CARTESIAN_POINT ( 'NONE',  ( 10.18405858231679417, -20.79840458871652942, 2.226721677130544030 ) ) ;
#18616 = DIRECTION ( 'NONE',  ( -0.000000000000000000, -0.000000000000000000, -1.000000000000000000 ) ) ;
#18617 = CARTESIAN_POINT ( 'NONE',  ( -13.40432071140796744, -19.51930407389869515, 6.223619713037471968 ) ) ;
#18618 = CARTESIAN_POINT ( 'NONE',  ( 10.74655858231679417, -21.94931252712234482, 5.250000000000000888 ) ) ;
#18619 = EDGE_CURVE ( 'NONE', #4544, #7379, #6335, .T. ) ;
#18620 = FACE_OUTER_BOUND ( 'NONE', #6935, .T. ) ;
#18621 = ORIENTED_EDGE ( 'NONE', *, *, #20498, .T. ) ;
#18622 = EDGE_CURVE ( 'NONE', #12851, #17198, #14267, .T. ) ;
#18623 = ORIENTED_EDGE ( 'NONE', *, *, #13710, .T. ) ;
#18624 = CARTESIAN_POINT ( 'NONE',  ( 13.37499999999998401, -20.99999999999999645, 3.666666666666654084 ) ) ;
#18625 = LINE ( 'NONE', #7634, #11471 ) ;
#18626 = DIRECTION ( 'NONE',  ( 0.000000000000000000, 0.000000000000000000, 1.000000000000000000 ) ) ;
#18627 = ORIENTED_EDGE ( 'NONE', *, *, #1472, .F. ) ;
#18628 = DIRECTION ( 'NONE',  ( 0.000000000000000000, 0.000000000000000000, 1.000000000000000000 ) ) ;
#18629 = VERTEX_POINT ( 'NONE', #12708 ) ;
#18630 = CARTESIAN_POINT ( 'NONE',  ( -10.18405858231679417, -20.79840458871652942, 2.226721677130544030 ) ) ;
#18631 = CARTESIAN_POINT ( 'NONE',  ( 13.87470602645761986, 4.985154336109792972, 4.791666666666685614 ) ) ;
#18632 = LINE ( 'NONE', #2835, #6149 ) ;
#18633 = CARTESIAN_POINT ( 'NONE',  ( 3.475298211275419380, -9.785109117490691233, 1.987377451789144933 ) ) ;
#18634 = EDGE_CURVE ( 'NONE', #5490, #18833, #4763, .T. ) ;
#18635 = CARTESIAN_POINT ( 'NONE',  ( -27.00000000000000000, 0.000000000000000000, 1.000000000000000000 ) ) ;
#18636 = CARTESIAN_POINT ( 'NONE',  ( -13.37939227869017600, -19.27818992614120575, 4.741950614318236390 ) ) ;
#18637 = DIRECTION ( 'NONE',  ( 1.000000000000000000, 0.000000000000000000, 0.000000000000000000 ) ) ;
#18638 = CARTESIAN_POINT ( 'NONE',  ( -13.40957725085194241, -19.25384883197511243, 6.242932005802575901 ) ) ;
#18639 = CARTESIAN_POINT ( 'NONE',  ( 11.00000000000000000, -18.49999999999999645, 6.500000000000000888 ) ) ;
#18640 = CARTESIAN_POINT ( 'NONE',  ( 11.77780858231679417, -20.27099543870833642, 2.724438792969431589 ) ) ;
#18641 = CARTESIAN_POINT ( 'NONE',  ( 10.47219141768317741, -22.97900456129165292, 3.035098964749240125 ) ) ;
#18642 = CARTESIAN_POINT ( 'NONE',  ( -6.152808582316793284, -21.22443879296942626, 5.229004561291659137 ) ) ;
#18643 = VERTEX_POINT ( 'NONE', #17517 ) ;
#18644 = CARTESIAN_POINT ( 'NONE',  ( 13.37499999999998224, -19.49999999999998934, 4.291666666666699825 ) ) ;
#18645 = PLANE ( 'NONE',  #5665 ) ;
#18646 = ORIENTED_EDGE ( 'NONE', *, *, #20385, .F. ) ;
#18647 = AXIS2_PLACEMENT_3D ( 'NONE', #18830, #6989, #2172 ) ;
#18648 = UNCERTAINTY_MEASURE_WITH_UNIT (LENGTH_MEASURE( 1.000000000000000082E-05 ), #2200, 'distance_accuracy_value', 'NONE');
#18649 = VERTEX_POINT ( 'NONE', #2442 ) ;
#18650 = CARTESIAN_POINT ( 'NONE',  ( 12.25209451496117197, 10.00000000000000000, 1.000000000000000000 ) ) ;
#18651 = CARTESIAN_POINT ( 'NONE',  ( -13.09892531043291086, 3.683228176858501790, 6.000681092915118420 ) ) ;
#18652 = FACE_OUTER_BOUND ( 'NONE', #9198, .T. ) ;
#18653 = CARTESIAN_POINT ( 'NONE',  ( -13.83065313257865370, 2.760483195222930952, 5.966304699623404595 ) ) ;
#18654 = EDGE_CURVE ( 'NONE', #4981, #68, #8427, .T. ) ;
#18655 = CARTESIAN_POINT ( 'NONE',  ( 10.00000000000000533, -30.00000000000000355, 1.000000000000000000 ) ) ;
#18656 = FACE_OUTER_BOUND ( 'NONE', #18836, .T. ) ;
#18657 = DIRECTION ( 'NONE',  ( 1.000000000000000000, 0.000000000000000000, 0.000000000000000000 ) ) ;
#18658 = PLANE ( 'NONE',  #10734 ) ;
#18659 = CARTESIAN_POINT ( 'NONE',  ( -11.99999999999999645, -26.49999999999998934, 4.000000000000000000 ) ) ;
#18660 = CARTESIAN_POINT ( 'NONE',  ( -11.59030858231679595, -21.01515356694490322, 0.9790045612916562501 ) ) ;
#18661 = CARTESIAN_POINT ( 'NONE',  ( -1.720709671993384093, -9.114925383610804843, 1.622645897908254753 ) ) ;
#18662 = ORIENTED_EDGE ( 'NONE', *, *, #11946, .T. ) ;
#18663 = CARTESIAN_POINT ( 'NONE',  ( -13.37597619100657198, -20.20070235416671167, 4.815535977982682070 ) ) ;
#18664 = DIRECTION ( 'NONE',  ( -1.000000000000000000, -0.000000000000000000, -0.000000000000000000 ) ) ;
#18665 = CARTESIAN_POINT ( 'NONE',  ( 10.94094141768317741, -20.19639159124061933, 1.768074502826635586 ) ) ;
#18666 = CARTESIAN_POINT ( 'NONE',  ( -4.190941417683176518, -23.27327832286946219, 4.701595411283453707 ) ) ;
#18667 = ORIENTED_EDGE ( 'NONE', *, *, #14598, .T. ) ;
#18668 = CARTESIAN_POINT ( 'NONE',  ( 13.87215786865436762, 4.856472367046606564, 5.506273593909547515 ) ) ;
#18669 = DIRECTION ( 'NONE',  ( -0.000000000000000000, 0.000000000000000000, -1.000000000000000000 ) ) ;
#18670 = VECTOR ( 'NONE', #3731, 1000.000000000000000 ) ;
#18671 = ORIENTED_EDGE ( 'NONE', *, *, #1030, .F. ) ;
#18672 = AXIS2_PLACEMENT_3D ( 'NONE', #4265, #5744, #12115 ) ;
#18673 = ORIENTED_EDGE ( 'NONE', *, *, #4875, .F. ) ;
#18674 = CARTESIAN_POINT ( 'NONE',  ( -14.49999999999998401, -25.49999999999999645, 4.000000000000000000 ) ) ;
#18675 = VECTOR ( 'NONE', #2339, 1000.000000000000000 ) ;
#18676 = ORIENTED_EDGE ( 'NONE', *, *, #5914, .F. ) ;
#18677 = LINE ( 'NONE', #4345, #9106 ) ;
#18678 = CARTESIAN_POINT ( 'NONE',  ( 2.567175533087980188, -9.771398394011347577, 2.541241281345096859 ) ) ;
#18679 = VECTOR ( 'NONE', #14279, 1000.000000000000000 ) ;
#18680 = VERTEX_POINT ( 'NONE', #11649 ) ;
#18681 = DIRECTION ( 'NONE',  ( -1.000000000000000000, -1.156482317317871331E-15, 0.000000000000000000 ) ) ;
#18682 = LINE ( 'NONE', #13446, #7675 ) ;
#18683 = DIRECTION ( 'NONE',  ( 0.000000000000000000, 1.000000000000000000, -0.000000000000000000 ) ) ;
#18684 = VECTOR ( 'NONE', #6327, 1000.000000000000000 ) ;
#18685 = CARTESIAN_POINT ( 'NONE',  ( 3.451003380014874722, -9.682417022083358304, 1.961004070207825523 ) ) ;
#18686 = CARTESIAN_POINT ( 'NONE',  ( 2.687849085826861995, 0.000000000000000000, 1.000000000000000000 ) ) ;
#18687 = CARTESIAN_POINT ( 'NONE',  ( 13.12529397353891270, 5.014845663890295846, 3.333333333333220239 ) ) ;
#18688 = EDGE_CURVE ( 'NONE', #18720, #17894, #14689, .T. ) ;
#18689 = VECTOR ( 'NONE', #9602, 1000.000000000000000 ) ;
#18690 = CARTESIAN_POINT ( 'NONE',  ( 14.50000000000000000, -20.99999999999998934, 4.000000000000000000 ) ) ;
#18691 = CARTESIAN_POINT ( 'NONE',  ( 3.469446951953523943E-14, 10.00000000000009592, 1.000000000000000000 ) ) ;
#18692 = DIRECTION ( 'NONE',  ( 0.000000000000000000, 0.000000000000000000, 1.000000000000000000 ) ) ;
#18693 = CARTESIAN_POINT ( 'NONE',  ( 5.597191417683177406, -22.46490103525075810, 4.479004561291653808 ) ) ;
#18694 = CARTESIAN_POINT ( 'NONE',  ( -13.10192273101908000, 3.834597916462216816, 6.003936301248457674 ) ) ;
#18695 = CARTESIAN_POINT ( 'NONE',  ( -10.93405858231679595, -22.67126532539354855, 4.242948236979545484 ) ) ;
#18696 = CARTESIAN_POINT ( 'NONE',  ( -4.687312169500634340, -21.32903648725300272, 5.908812401261035241 ) ) ;
#18697 = EDGE_LOOP ( 'NONE', ( #20606, #20589, #10104, #12915 ) ) ;
#18698 = ADVANCED_FACE ( 'NONE', ( #8733 ), #6949, .T. ) ;
#18699 = CARTESIAN_POINT ( 'NONE',  ( 12.63118877378512828, -19.18746692385052555, 4.758813856674282583 ) ) ;
#18700 = CARTESIAN_POINT ( 'NONE',  ( -13.12526104302547836, 5.013182672784613381, 5.066812735559260261 ) ) ;
#18701 = ORIENTED_EDGE ( 'NONE', *, *, #14739, .F. ) ;
#18702 = EDGE_CURVE ( 'NONE', #5682, #17800, #15101, .T. ) ;
#18703 = DIRECTION ( 'NONE',  ( 0.000000000000000000, 1.000000000000000000, -0.000000000000000000 ) ) ;
#18704 = ORIENTED_EDGE ( 'NONE', *, *, #9541, .F. ) ;
#18705 = CARTESIAN_POINT ( 'NONE',  ( 2.567175533087980188, -9.771398394011347577, 2.541241281345096859 ) ) ;
#18706 = APPLICATION_CONTEXT ( 'automotive_design' ) ;
#18707 = AXIS2_PLACEMENT_3D ( 'NONE', #4260, #9459, #7890 ) ;
#18708 = ORIENTED_EDGE ( 'NONE', *, *, #553, .T. ) ;
#18709 = CARTESIAN_POINT ( 'NONE',  ( -0.1250000000000001110, 0.000000000000000000, 0.000000000000000000 ) ) ;
#18710 = LINE ( 'NONE', #18505, #12966 ) ;
#18711 = CIRCLE ( 'NONE', #18047, 0.5000000000000000000 ) ;
#18712 = CARTESIAN_POINT ( 'NONE',  ( -1.337453470010121714, -9.864917468222230923, 1.622643865078341907 ) ) ;
#18713 = CARTESIAN_POINT ( 'NONE',  ( -18.69064177244175795, 10.00000000000000000, 1.000000000000000000 ) ) ;
#18714 = LINE ( 'NONE', #18820, #8966 ) ;
#18715 = EDGE_CURVE ( 'NONE', #19461, #6659, #2235, .T. ) ;
#18716 = DIRECTION ( 'NONE',  ( 0.000000000000000000, 0.000000000000000000, 1.000000000000000000 ) ) ;
#18717 = CARTESIAN_POINT ( 'NONE',  ( 5.128441417683177406, -19.49999999999998934, 3.550687472877664952 ) ) ;
#18718 = FACE_BOUND ( 'NONE', #9786, .T. ) ;
#18719 = CARTESIAN_POINT ( 'NONE',  ( -7.940941417683176518, -20.72672167713052715, 2.298404588716546293 ) ) ;
#18720 = VERTEX_POINT ( 'NONE', #13319 ) ;
#18721 = CARTESIAN_POINT ( 'NONE',  ( 8.965308582316794173, -20.22900456129164937, 4.174186261275266929 ) ) ;
#18722 = CARTESIAN_POINT ( 'NONE',  ( 11.00000000000000000, -25.49999999999999645, 6.500000000000000000 ) ) ;
#18723 = CARTESIAN_POINT ( 'NONE',  ( -13.37499999999998224, -21.00000000000006395, 4.416666666666682062 ) ) ;
#18724 = ORIENTED_EDGE ( 'NONE', *, *, #16428, .T. ) ;
#18725 = AXIS2_PLACEMENT_3D ( 'NONE', #3469, #5142, #9947 ) ;
#18726 = CARTESIAN_POINT ( 'NONE',  ( 12.90280858231679773, -22.77556120703056308, 1.770995438708339975 ) ) ;
#18727 = DIRECTION ( 'NONE',  ( 1.000000000000000000, 0.000000000000000000, 0.000000000000000000 ) ) ;
#18728 = EDGE_LOOP ( 'NONE', ( #15774, #13414, #4030, #17126 ) ) ;
#18729 = ORIENTED_EDGE ( 'NONE', *, *, #16143, .F. ) ;
#18730 = CARTESIAN_POINT ( 'NONE',  ( 13.40995420747273670, -19.23481252262645924, 6.243328185864100988 ) ) ;
#18731 = CARTESIAN_POINT ( 'NONE',  ( 0.000000000000000000, 4.999999999999999112, 0.000000000000000000 ) ) ;
#18732 =( LENGTH_UNIT ( ) NAMED_UNIT ( * ) SI_UNIT ( .MILLI., .METRE. ) );
#18733 = ORIENTED_EDGE ( 'NONE', *, *, #1281, .F. ) ;
#18734 = LINE ( 'NONE', #7541, #19493 ) ;
#18735 = ORIENTED_EDGE ( 'NONE', *, *, #16817, .T. ) ;
#18736 = CARTESIAN_POINT ( 'NONE',  ( -10.37155858231679417, -20.24999999999999289, 3.449312527122348371 ) ) ;
#18737 = PLANE ( 'NONE',  #18957 ) ;
#18738 = CARTESIAN_POINT ( 'NONE',  ( 7.499999999999999112, -18.49999999999999645, 6.500000000000000888 ) ) ;
#18739 = CARTESIAN_POINT ( 'NONE',  ( 3.502569552650398155, -9.961070227720959736, 2.032567780072621400 ) ) ;
#18740 = VECTOR ( 'NONE', #12917, 1000.000000000000000 ) ;
#18741 = AXIS2_PLACEMENT_3D ( 'NONE', #7478, #2548, #16979 ) ;
#18742 = ADVANCED_FACE ( 'NONE', ( #4017 ), #13123, .F. ) ;
#18743 = EDGE_CURVE ( 'NONE', #13273, #9411, #9980, .T. ) ;
#18744 = LINE ( 'NONE', #15584, #2041 ) ;
#18745 = CARTESIAN_POINT ( 'NONE',  ( -13.09206359972826661, 4.086711786274932479, 5.245812454509717782 ) ) ;
#18746 = CARTESIAN_POINT ( 'NONE',  ( 10.46530858231679417, -20.22900456129164937, 4.174186261275266929 ) ) ;
#18747 = CARTESIAN_POINT ( 'NONE',  ( -13.37499999999998224, -20.99999999999998934, 4.166666666666637653 ) ) ;
#18748 = CARTESIAN_POINT ( 'NONE',  ( 27.44203811574919882, 16.00000000000000000, 1.000000000000000000 ) ) ;
#18749 = CARTESIAN_POINT ( 'NONE',  ( 11.68405858231679417, -20.79840458871652942, 2.226721677130544030 ) ) ;
#18750 = CARTESIAN_POINT ( 'NONE',  ( 3.974842109207561425, -21.82955800590261575, 5.256404853634145447 ) ) ;
#18751 = CARTESIAN_POINT ( 'NONE',  ( -11.03469141768317918, -20.22900456129164581, 2.825813738724748170 ) ) ;
#18752 = VERTEX_POINT ( 'NONE', #5273 ) ;
#18753 = CARTESIAN_POINT ( 'NONE',  ( 13.39169183355864590, -18.65706240528901105, 4.755687463382285429 ) ) ;
#18754 = VECTOR ( 'NONE', #11103, 1000.000000000000000 ) ;
#18755 = DIRECTION ( 'NONE',  ( -1.000000000000000000, 0.000000000000000000, 0.000000000000000000 ) ) ;
#18756 = ORIENTED_EDGE ( 'NONE', *, *, #664, .T. ) ;
#18757 = AXIS2_PLACEMENT_3D ( 'NONE', #5246, #5355, #19391 ) ;
#18758 = AXIS2_PLACEMENT_3D ( 'NONE', #2958, #17701, #15712 ) ;
#18759 = ORIENTED_EDGE ( 'NONE', *, *, #14329, .F. ) ;
#18760 = FACE_OUTER_BOUND ( 'NONE', #10753, .T. ) ;
#18761 = VECTOR ( 'NONE', #16480, 1000.000000000000000 ) ;
#18762 = CARTESIAN_POINT ( 'NONE',  ( -12.83635126708105823, -9.576761012430582198, 5.715524842913705328 ) ) ;
#18763 = CARTESIAN_POINT ( 'NONE',  ( -2.513306525444908512, -9.622685169956881168, 2.503048754562789746 ) ) ;
#18764 = CARTESIAN_POINT ( 'NONE',  ( -13.87470602645761986, 4.985154336109792972, 4.791666666666685614 ) ) ;
#18765 = DIRECTION ( 'NONE',  ( 0.000000000000000000, 0.000000000000000000, -1.000000000000000000 ) ) ;
#18766 = CARTESIAN_POINT ( 'NONE',  ( 7.499999999999999112, -20.16506350946107418, 5.250000000000000000 ) ) ;
#18767 = CARTESIAN_POINT ( 'NONE',  ( 11.49178095869207006, 9.000000000000001776, 1.000000000000000000 ) ) ;
#18768 = CARTESIAN_POINT ( 'NONE',  ( 21.25349085826861995, 11.64110105645932691, 0.000000000000000000 ) ) ;
#18769 = DIRECTION ( 'NONE',  ( 1.000000000000000000, 0.000000000000000000, -0.000000000000000000 ) ) ;
#18770 = CARTESIAN_POINT ( 'NONE',  ( -10.65280858231679595, -20.91377862118960351, 5.979004561291660913 ) ) ;
#18771 = VECTOR ( 'NONE', #2054, 1000.000000000000000 ) ;
#18772 = CARTESIAN_POINT ( 'NONE',  ( 0.000000000000000000, -8.364917468222230923, 1.622643865078341241 ) ) ;
#18773 = ORIENTED_EDGE ( 'NONE', *, *, #6891, .T. ) ;
#18774 = CARTESIAN_POINT ( 'NONE',  ( -13.37500015856764435, -20.24999199233421265, 4.532157119432948633 ) ) ;
#18775 = DIRECTION ( 'NONE',  ( -0.000000000000000000, -0.000000000000000000, -1.000000000000000000 ) ) ;
#18776 = CARTESIAN_POINT ( 'NONE',  ( 10.47219141768317741, -24.47900456129165292, 2.413778621189595963 ) ) ;
#18777 = CARTESIAN_POINT ( 'NONE',  ( -5.597191417683177406, -22.46490103525075810, 4.479004561291653808 ) ) ;
#18778 = ORIENTED_EDGE ( 'NONE', *, *, #20608, .T. ) ;
#18779 = CARTESIAN_POINT ( 'NONE',  ( 13.37607268932110038, -20.94582918928111681, 4.945564004704174010 ) ) ;
#18780 = PLANE ( 'NONE',  #10057 ) ;
#18781 = ORIENTED_EDGE ( 'NONE', *, *, #8231, .F. ) ;
#18782 = ORIENTED_EDGE ( 'NONE', *, *, #4087, .F. ) ;
#18783 = EDGE_CURVE ( 'NONE', #13004, #15521, #11639, .T. ) ;
#18784 = DIRECTION ( 'NONE',  ( 0.000000000000000000, 0.000000000000000000, -1.000000000000000000 ) ) ;
#18785 = ORIENTED_EDGE ( 'NONE', *, *, #5592, .T. ) ;
#18786 = DIRECTION ( 'NONE',  ( 0.000000000000000000, -0.000000000000000000, 1.000000000000000000 ) ) ;
#18787 = VECTOR ( 'NONE', #8002, 1000.000000000000000 ) ;
#18788 = DIRECTION ( 'NONE',  ( 0.000000000000000000, 1.000000000000000000, 0.000000000000000000 ) ) ;
#18789 = EDGE_LOOP ( 'NONE', ( #10928, #15548, #5835, #11034 ) ) ;
#18790 = CARTESIAN_POINT ( 'NONE',  ( -4.000000000000000000, -12.50000000000000000, 1.000000000000000000 ) ) ;
#18791 = DIRECTION ( 'NONE',  ( -0.000000000000000000, -0.000000000000000000, -1.000000000000000000 ) ) ;
#18792 = CARTESIAN_POINT ( 'NONE',  ( -11.74178095869206828, 9.000000000000001776, 1.000000000000000000 ) ) ;
#18793 = CARTESIAN_POINT ( 'NONE',  ( 1.798207051321043304, -8.367281747657623114, 1.623251059268568053 ) ) ;
#18794 = FACE_OUTER_BOUND ( 'NONE', #4161, .T. ) ;
#18795 = CARTESIAN_POINT ( 'NONE',  ( 13.10624331898488037, 4.052787608736739600, 6.006964772046813117 ) ) ;
#18796 = VECTOR ( 'NONE', #6015, 1000.000000000000000 ) ;
#18797 = DIRECTION ( 'NONE',  ( -0.000000000000000000, -0.000000000000000000, -1.000000000000000000 ) ) ;
#18798 = CARTESIAN_POINT ( 'NONE',  ( -24.12918902992234393, 0.000000000000000000, 1.000000000000000000 ) ) ;
#18799 = DIRECTION ( 'NONE',  ( -1.156482317317871133E-15, 1.000000000000000000, 0.000000000000000000 ) ) ;
#18800 = CARTESIAN_POINT ( 'NONE',  ( 8.315941417683177406, -21.32873467460645145, 4.242948236979555254 ) ) ;
#18801 = CARTESIAN_POINT ( 'NONE',  ( -12.65051119073526564, -18.96168486786632457, 5.513701926248478102 ) ) ;
#18802 = CARTESIAN_POINT ( 'NONE',  ( -13.18405858231679595, -21.32873467460644079, 2.757051763020455404 ) ) ;
#18803 = VECTOR ( 'NONE', #18138, 1000.000000000000000 ) ;
#18804 = CARTESIAN_POINT ( 'NONE',  ( -4.753441417683176518, -21.94931252712233061, 0.9999999999999978906 ) ) ;
#18805 = ORIENTED_EDGE ( 'NONE', *, *, #15949, .F. ) ;
#18806 = CARTESIAN_POINT ( 'NONE',  ( 13.37523871602689596, -19.48794484064217514, 4.577160611493482634 ) ) ;
#18807 = DIRECTION ( 'NONE',  ( -0.000000000000000000, -0.000000000000000000, -1.000000000000000000 ) ) ;
#18808 = ORIENTED_EDGE ( 'NONE', *, *, #9614, .T. ) ;
#18809 = FACE_OUTER_BOUND ( 'NONE', #6905, .T. ) ;
#18810 = VERTEX_POINT ( 'NONE', #778 ) ;
#18811 = CARTESIAN_POINT ( 'NONE',  ( 1.896776615114361908, -10.21987218505477024, 2.463803327293850209 ) ) ;
#18812 = EDGE_CURVE ( 'NONE', #3441, #10513, #5483, .T. ) ;
#18813 = ORIENTED_EDGE ( 'NONE', *, *, #10725, .F. ) ;
#18814 = DIRECTION ( 'NONE',  ( 0.7071067811865474617, -0.000000000000000000, 0.7071067811865474617 ) ) ;
#18815 = CIRCLE ( 'NONE', #2790, 0.3749999999999997224 ) ;
#18816 = CARTESIAN_POINT ( 'NONE',  ( -29.71062960567704891, 11.64110105645932691, -1.734723475976807094E-15 ) ) ;
#18817 = ADVANCED_FACE ( 'NONE', ( #3601 ), #673, .T. ) ;
#18818 = CARTESIAN_POINT ( 'NONE',  ( -2.627360420079438263, -14.25085146736906339, 2.749039333894452763 ) ) ;
#18819 = PLANE ( 'NONE',  #16998 ) ;
#18820 = CARTESIAN_POINT ( 'NONE',  ( 0.000000000000000000, 9.000000000000001776, 0.000000000000000000 ) ) ;
#18821 = EDGE_CURVE ( 'NONE', #17687, #6665, #14794, .T. ) ;
#18822 = DIRECTION ( 'NONE',  ( -1.000000000000000000, -0.000000000000000000, -0.000000000000000000 ) ) ;
#18823 = CARTESIAN_POINT ( 'NONE',  ( 6.628441417683177406, -19.49999999999998934, 3.550687472877664952 ) ) ;
#18824 =( NAMED_UNIT ( * ) SI_UNIT ( $, .STERADIAN. ) SOLID_ANGLE_UNIT ( ) );
#18825 = CARTESIAN_POINT ( 'NONE',  ( -8.878441417683177406, -23.74999999999999645, 3.449312527122335492 ) ) ;
#18826 = EDGE_LOOP ( 'NONE', ( #15190, #2385, #8789, #5760 ) ) ;
#18827 = CARTESIAN_POINT ( 'NONE',  ( 7.371558582316794173, -20.24999999999999289, 3.449312527122348371 ) ) ;
#18828 = DIRECTION ( 'NONE',  ( 0.000000000000000000, -0.000000000000000000, 1.000000000000000000 ) ) ;
#18829 = CARTESIAN_POINT ( 'NONE',  ( -12.62499999999998224, -20.99999999999998934, 4.291666666666699825 ) ) ;
#18830 = CARTESIAN_POINT ( 'NONE',  ( -9.689245429134309973, 0.000000000000000000, 1.000000000000000000 ) ) ;
#18831 = PLANE ( 'NONE',  #13328 ) ;
#18832 = EDGE_LOOP ( 'NONE', ( #11863, #8327, #12086, #13778 ) ) ;
#18833 = VERTEX_POINT ( 'NONE', #18352 ) ;
#18834 = CARTESIAN_POINT ( 'NONE',  ( 13.83079205777725917, 2.017498917744843023, 6.700359435863729729 ) ) ;
#18835 = CARTESIAN_POINT ( 'NONE',  ( 4.247260319564023945, 9.000000000000001776, 1.000000000000000000 ) ) ;
#18836 = EDGE_LOOP ( 'NONE', ( #16274, #17795, #20240, #685 ) ) ;
#18837 = EDGE_CURVE ( 'NONE', #9910, #13028, #10106, .T. ) ;
#18838 = PLANE ( 'NONE',  #2112 ) ;
#18839 = ORIENTED_EDGE ( 'NONE', *, *, #19803, .F. ) ;
#18840 = CARTESIAN_POINT ( 'NONE',  ( -13.09030858231679417, -21.32581373872472597, 1.729004561291657582 ) ) ;
#18841 = CARTESIAN_POINT ( 'NONE',  ( 0.000000000000000000, 4.999999999999999112, 1.000000000000000000 ) ) ;
#18842 = AXIS2_PLACEMENT_3D ( 'NONE', #12871, #11411, #18784 ) ;
#18843 = EDGE_CURVE ( 'NONE', #17840, #19958, #10502, .T. ) ;
#18844 = DIRECTION ( 'NONE',  ( 0.1351665943404306014, -0.9596796555888912339, 0.2464649070825229438 ) ) ;
#18845 = CARTESIAN_POINT ( 'NONE',  ( 1.652577328807104839, -9.114908150887895744, 1.622641472200749835 ) ) ;
#18846 = EDGE_CURVE ( 'NONE', #6462, #19322, #3618, .T. ) ;
#18847 = FACE_OUTER_BOUND ( 'NONE', #4187, .T. ) ;
#18848 = CARTESIAN_POINT ( 'NONE',  ( -13.09533517714100093, 4.251926445620864747, 5.084080158857392284 ) ) ;
#18849 = CARTESIAN_POINT ( 'NONE',  ( 9.715308582316794173, -23.77099543870833998, 2.825813738724734847 ) ) ;
#18850 = CARTESIAN_POINT ( 'NONE',  ( -13.87372783958217681, 4.185755898898970706, 6.732634959205082481 ) ) ;
#18851 = PLANE ( 'NONE',  #12065 ) ;
#18852 = CARTESIAN_POINT ( 'NONE',  ( 7.277808582316794173, -20.27099543870833642, 2.724438792969431589 ) ) ;
#18853 = AXIS2_PLACEMENT_3D ( 'NONE', #14989, #667, #5480 ) ;
#18854 = CARTESIAN_POINT ( 'NONE',  ( 4.940941417683177406, -20.72672167713052715, 2.298404588716546293 ) ) ;
#18855 = CARTESIAN_POINT ( 'NONE',  ( -7.652808582316795061, -21.22443879296942626, 5.229004561291659137 ) ) ;
#18856 = ORIENTED_EDGE ( 'NONE', *, *, #14523, .T. ) ;
#18857 = CARTESIAN_POINT ( 'NONE',  ( 13.37514942709654164, -19.49245393162283690, 4.562067678168288509 ) ) ;
#18858 = CARTESIAN_POINT ( 'NONE',  ( 4.000000000000000000, -8.500000000000000000, 2.392927049865408495 ) ) ;
#18859 = ORIENTED_EDGE ( 'NONE', *, *, #1611, .F. ) ;
#18860 = EDGE_CURVE ( 'NONE', #11896, #13228, #10600, .T. ) ;
#18861 = ORIENTED_EDGE ( 'NONE', *, *, #6674, .T. ) ;
#18862 = LINE ( 'NONE', #10908, #14112 ) ;
#18863 = CARTESIAN_POINT ( 'NONE',  ( -13.10252221513633941, 3.864871864382954048, 6.004587342915129966 ) ) ;
#18864 = PRODUCT ( 'Fixed Lower Stainless Steel Comb Blade', 'Fixed Lower Stainless Steel Comb Blade', '', ( #18501 ) ) ;
#18865 = CARTESIAN_POINT ( 'NONE',  ( -1.728780693989796724, -8.364929292255887106, 2.372646901726390478 ) ) ;
#18866 = CARTESIAN_POINT ( 'NONE',  ( -13.85163507668220539, 3.820071372449974412, 5.989091157956555556 ) ) ;
#18867 = CARTESIAN_POINT ( 'NONE',  ( 3.499999999999998668, -19.50000000000000000, 1.000000000000000000 ) ) ;
#18868 = LINE ( 'NONE', #1289, #19235 ) ;
#18869 = CARTESIAN_POINT ( 'NONE',  ( -15.87779268661489773, 16.00000000000000000, 1.000000000000000000 ) ) ;
#18870 = LINE ( 'NONE', #17704, #12396 ) ;
#18871 = EDGE_CURVE ( 'NONE', #20090, #9554, #2627, .T. ) ;
#18872 = CARTESIAN_POINT ( 'NONE',  ( -4.717959273841178636, -21.72818306014730183, 5.243595146365860771 ) ) ;
#18873 = CARTESIAN_POINT ( 'NONE',  ( -1.733187991654075777, -9.867296153774269385, 1.623254759047128237 ) ) ;
#18874 = ORIENTED_EDGE ( 'NONE', *, *, #15642, .T. ) ;
#18875 = CARTESIAN_POINT ( 'NONE',  ( -13.84042474920106081, 4.003949834653575124, 5.242612001278796008 ) ) ;
#18876 = PLANE ( 'NONE',  #20423 ) ;
#18877 = CARTESIAN_POINT ( 'NONE',  ( 6.996558582316795949, -22.05068747287764452, 0.9999999999999978906 ) ) ;
#18878 = CARTESIAN_POINT ( 'NONE',  ( -11.77780858231679595, -21.02099543870833998, 3.035098964749253003 ) ) ;
#18879 = ORIENTED_EDGE ( 'NONE', *, *, #3482, .T. ) ;
#18880 = CARTESIAN_POINT ( 'NONE',  ( 13.87470623115321899, 4.985164673244912414, 4.958488177337359026 ) ) ;
#18881 = DIRECTION ( 'NONE',  ( 0.000000000000000000, 1.000000000000000000, -0.000000000000000000 ) ) ;
#18882 = EDGE_LOOP ( 'NONE', ( #18500, #20376, #13220, #2179 ) ) ;
#18883 = ORIENTED_EDGE ( 'NONE', *, *, #10029, .T. ) ;
#18884 = LINE ( 'NONE', #1693, #13107 ) ;
#18885 = EDGE_CURVE ( 'NONE', #6147, #4809, #16974, .T. ) ;
#18886 = ORIENTED_EDGE ( 'NONE', *, *, #4807, .T. ) ;
#18887 = EDGE_CURVE ( 'NONE', #1368, #4053, #13933, .T. ) ;
#18888 = CARTESIAN_POINT ( 'NONE',  ( -13.87470602645761986, 4.985154336109792972, 4.166666666666758445 ) ) ;
#18889 = VECTOR ( 'NONE', #440, 1000.000000000000000 ) ;
#18890 = CARTESIAN_POINT ( 'NONE',  ( 1.548630333695928396, -9.114917468222230923, 2.372643865078341019 ) ) ;
#18891 = EDGE_CURVE ( 'NONE', #15348, #9078, #1192, .T. ) ;
#18892 = ORIENTED_EDGE ( 'NONE', *, *, #5174, .T. ) ;
#18893 = LINE ( 'NONE', #4552, #14865 ) ;
#18894 = CARTESIAN_POINT ( 'NONE',  ( 2.567175533087980188, -9.771398394011347577, 2.541241281345096859 ) ) ;
#18895 = DIRECTION ( 'NONE',  ( 1.000000000000000000, 0.000000000000000000, 0.000000000000000000 ) ) ;
#18896 = CARTESIAN_POINT ( 'NONE',  ( 1.948765222931501784, -9.143197003266354983, 1.629906614618163552 ) ) ;
#18897 = DIRECTION ( 'NONE',  ( 5.204170427930411817E-15, -1.000000000000000000, 0.000000000000000000 ) ) ;
#18898 = CARTESIAN_POINT ( 'NONE',  ( 6.063547257480584207, 11.64110105645932691, 0.000000000000000000 ) ) ;
#18899 = EDGE_CURVE ( 'NONE', #3823, #15395, #980, .T. ) ;
#18900 = CARTESIAN_POINT ( 'NONE',  ( -14.49999999999998579, -21.99999999999999645, 12.00000000000000355 ) ) ;
#18901 = FACE_OUTER_BOUND ( 'NONE', #9250, .T. ) ;
#18902 = LINE ( 'NONE', #17212, #19709 ) ;
#18903 = CIRCLE ( 'NONE', #9870, 59.99999999999998579 ) ;
#18904 = CARTESIAN_POINT ( 'NONE',  ( 6.909691417683176518, -21.63647391050456648, 4.520995438708348857 ) ) ;
#18905 = CARTESIAN_POINT ( 'NONE',  ( -12.62499999999998401, -19.49999999999998934, 3.666666666666654084 ) ) ;
#18906 = CARTESIAN_POINT ( 'NONE',  ( -10.18405858231679595, -21.32873467460644079, 2.757051763020455404 ) ) ;
#18907 = CARTESIAN_POINT ( 'NONE',  ( -11.22219141768317741, -20.27099543870833998, 4.275561207030583510 ) ) ;
#18908 = ORIENTED_EDGE ( 'NONE', *, *, #10183, .F. ) ;
#18909 = CARTESIAN_POINT ( 'NONE',  ( 13.08080186171710224, 3.517994016715657146, 5.247095106674282583 ) ) ;
#18910 = LINE ( 'NONE', #9274, #8981 ) ;
#18911 = EDGE_LOOP ( 'NONE', ( #11493, #3616, #7674, #7931 ) ) ;
#18912 = CARTESIAN_POINT ( 'NONE',  ( 0.000000000000000000, 0.000000000000000000, 1.000000000000000000 ) ) ;
#18913 = ORIENTED_EDGE ( 'NONE', *, *, #14537, .F. ) ;
#18914 = CARTESIAN_POINT ( 'NONE',  ( 1.837882866761050282, -9.938290523052360825, 2.391487531332776140 ) ) ;
#18915 = EDGE_LOOP ( 'NONE', ( #11992, #17175, #16225, #19764, #5133, #8557 ) ) ;
#18916 = CARTESIAN_POINT ( 'NONE',  ( 8.503441417683177406, -22.05068747287765873, 5.250000000000000888 ) ) ;
#18917 = LINE ( 'NONE', #19023, #10319 ) ;
#18918 = CARTESIAN_POINT ( 'NONE',  ( -1.407845757905374695, -9.864917468222230923, 1.622643865078341907 ) ) ;
#18919 = CARTESIAN_POINT ( 'NONE',  ( -14.49999999999999645, -21.00000000000000355, 1.000000000000000000 ) ) ;
#18920 = DIRECTION ( 'NONE',  ( 0.000000000000000000, 1.000000000000000000, -0.000000000000000000 ) ) ;
#18921 = EDGE_CURVE ( 'NONE', #19883, #4642, #10819, .T. ) ;
#18922 = DIRECTION ( 'NONE',  ( 0.000000000000000000, 1.000000000000000000, 0.000000000000000000 ) ) ;
#18923 = CARTESIAN_POINT ( 'NONE',  ( 7.753441417683177406, -21.94931252712233061, 0.9999999999999978906 ) ) ;
#18924 = FACE_OUTER_BOUND ( 'NONE', #1722, .T. ) ;
#18925 = CARTESIAN_POINT ( 'NONE',  ( -7.003441417683177406, -22.05068747287765873, 5.250000000000000888 ) ) ;
#18926 = ADVANCED_FACE ( 'NONE', ( #4435 ), #12375, .T. ) ;
#18927 = ORIENTED_EDGE ( 'NONE', *, *, #14910, .F. ) ;
#18928 = CARTESIAN_POINT ( 'NONE',  ( 9.902808582316794173, -22.77556120703056308, 1.770995438708339975 ) ) ;
#18929 = CARTESIAN_POINT ( 'NONE',  ( 0.000000000000000000, 10.00000000000000000, 1.000000000000000000 ) ) ;
#18930 = CARTESIAN_POINT ( 'NONE',  ( -12.62500000000002132, -21.00000000000274269, 4.083333333315724012 ) ) ;
#18931 = ORIENTED_EDGE ( 'NONE', *, *, #17075, .F. ) ;
#18932 = DIRECTION ( 'NONE',  ( 0.000000000000000000, 1.000000000000000000, -0.000000000000000000 ) ) ;
#18933 = DIRECTION ( 'NONE',  ( -0.000000000000000000, 0.000000000000000000, -1.000000000000000000 ) ) ;
#18934 = ORIENTED_EDGE ( 'NONE', *, *, #1360, .T. ) ;
#18935 = CARTESIAN_POINT ( 'NONE',  ( 13.49999999999998401, -25.49999999999999645, 4.000000000000000000 ) ) ;
#18936 =( NAMED_UNIT ( * ) SI_UNIT ( $, .STERADIAN. ) SOLID_ANGLE_UNIT ( ) );
#18937 = ORIENTED_EDGE ( 'NONE', *, *, #1049, .T. ) ;
#18938 = DIRECTION ( 'NONE',  ( -0.000000000000000000, -0.000000000000000000, -1.000000000000000000 ) ) ;
#18939 = ORIENTED_EDGE ( 'NONE', *, *, #13338, .T. ) ;
#18940 = CARTESIAN_POINT ( 'NONE',  ( -9.902808582316794173, -22.77556120703056308, 1.770995438708339975 ) ) ;
#18941 = CARTESIAN_POINT ( 'NONE',  ( 12.63465172146706728, -19.76258806590802664, 5.372658420469845986 ) ) ;
#18942 = CARTESIAN_POINT ( 'NONE',  ( 4.000698171653723101, 0.000000000000000000, 0.000000000000000000 ) ) ;
#18943 = CARTESIAN_POINT ( 'NONE',  ( 1.513434189748285696, -9.114917468222230923, 1.622643865078341463 ) ) ;
#18944 = CARTESIAN_POINT ( 'NONE',  ( -15.00000000000000000, 0.000000000000000000, 2.000000000000000000 ) ) ;
#18945 = VECTOR ( 'NONE', #5668, 1000.000000000000000 ) ;
#18946 = CARTESIAN_POINT ( 'NONE',  ( -13.37593719518949698, -19.45267164293252193, 4.647380496992003174 ) ) ;
#18947 = CARTESIAN_POINT ( 'NONE',  ( 6.340308582316793284, -22.67418626127525982, 5.270995438708342640 ) ) ;
#18948 = CARTESIAN_POINT ( 'NONE',  ( -12.62499999999998224, -21.00000000000006395, 4.416666666666682062 ) ) ;
#18949 = ADVANCED_FACE ( 'NONE', ( #2762 ), #9140, .T. ) ;
#18950 = DIRECTION ( 'NONE',  ( -0.000000000000000000, 0.000000000000000000, 1.000000000000000000 ) ) ;
#18951 = CARTESIAN_POINT ( 'NONE',  ( 6.527808582316794173, -23.72900456129165647, 4.275561207030568411 ) ) ;
#18952 = CARTESIAN_POINT ( 'NONE',  ( 7.753441417683177406, -21.94931252712233061, 2.499999999999999112 ) ) ;
#18953 = CARTESIAN_POINT ( 'NONE',  ( -10.84719141768317741, -21.22443879296941915, 1.770995438708345748 ) ) ;
#18954 = ORIENTED_EDGE ( 'NONE', *, *, #12553, .F. ) ;
#18955 = EDGE_CURVE ( 'NONE', #4851, #7250, #15609, .T. ) ;
#18956 = CARTESIAN_POINT ( 'NONE',  ( 13.37593719518949698, -19.45267164293252193, 4.647380496992003174 ) ) ;
#18958 = EDGE_CURVE ( 'NONE', #13385, #2700, #636, .T. ) ;
#18957 = AXIS2_PLACEMENT_3D ( 'NONE', #4404, #10383, #6386 ) ;
#18959 = CARTESIAN_POINT ( 'NONE',  ( -0.2815691515810352930, -9.114917468222230923, 1.622643865078524206 ) ) ;
#18960 = VERTEX_POINT ( 'NONE', #10475 ) ;
#18961 = ORIENTED_EDGE ( 'NONE', *, *, #20162, .F. ) ;
#18962 = FACE_OUTER_BOUND ( 'NONE', #198, .T. ) ;
#18963 = CIRCLE ( 'NONE', #9931, 10.00000000000000000 ) ;
#18964 = DIRECTION ( 'NONE',  ( -4.625929269271477434E-15, -1.000000000000000000, 0.000000000000000000 ) ) ;
#18965 = CARTESIAN_POINT ( 'NONE',  ( -3.321934647848983957, -9.834888441627915867, 2.750161776669472591 ) ) ;
#18966 = CARTESIAN_POINT ( 'NONE',  ( -13.85343352903393388, 3.910893216212274925, 5.991044282956552891 ) ) ;
#18967 = CARTESIAN_POINT ( 'NONE',  ( 2.762374231067749708, -9.968169115173667549, 1.841775933429679268 ) ) ;
#18968 = DIRECTION ( 'NONE',  ( 1.000000000000000000, -0.000000000000000000, -0.000000000000000000 ) ) ;
#18969 = CARTESIAN_POINT ( 'NONE',  ( 11.96530858231679417, -20.22900456129164937, 4.174186261275266929 ) ) ;
#18970 = VECTOR ( 'NONE', #15790, 1000.000000000000000 ) ;
#18971 = CARTESIAN_POINT ( 'NONE',  ( 17.30017143803810242, 0.000000000000000000, 1.000000000000000000 ) ) ;
#18972 = CARTESIAN_POINT ( 'NONE',  ( 13.15498501280115917, 5.764243146453090105, 5.045733045595949484 ) ) ;
#18973 = ADVANCED_FACE ( 'NONE', ( #3781 ), #5553, .T. ) ;
#18974 = CARTESIAN_POINT ( 'NONE',  ( -5.777808582316795949, -19.52099543870833642, 2.413778621189609286 ) ) ;
#18975 = CARTESIAN_POINT ( 'NONE',  ( -1.732184490400474175, -9.869581059509965115, 2.373841568485653308 ) ) ;
#18976 = ORIENTED_EDGE ( 'NONE', *, *, #184, .T. ) ;
#18977 = CARTESIAN_POINT ( 'NONE',  ( -13.38238173943565990, -19.87722215849730034, 5.285856107751903288 ) ) ;
#18978 = PLANE ( 'NONE',  #6049 ) ;
#18979 = VECTOR ( 'NONE', #17967, 1000.000000000000000 ) ;
#18980 = CARTESIAN_POINT ( 'NONE',  ( 5.222191417683177406, -19.52099543870834353, 4.586221378810406257 ) ) ;
#18981 = CARTESIAN_POINT ( 'NONE',  ( -4.284691417683177406, -23.02099543870834353, 3.863526089495429972 ) ) ;
#18982 = ORIENTED_EDGE ( 'NONE', *, *, #19098, .F. ) ;
#18983 = CARTESIAN_POINT ( 'NONE',  ( 13.39995901559228031, -19.73956971259024229, 6.178279423016713956 ) ) ;
#18984 = CARTESIAN_POINT ( 'NONE',  ( 14.00000000000000000, 7.806255641895631925E-15, 1.000000000000000000 ) ) ;
#18985 = LINE ( 'NONE', #11033, #10005 ) ;
#18986 = ORIENTED_EDGE ( 'NONE', *, *, #11038, .F. ) ;
#18987 = ORIENTED_EDGE ( 'NONE', *, *, #18958, .F. ) ;
#18988 = DIRECTION ( 'NONE',  ( -0.000000000000000000, -1.000000000000000000, -0.000000000000000000 ) ) ;
#18989 = CARTESIAN_POINT ( 'NONE',  ( 1.619022621591187150, -9.114917468222230923, 2.372643865078341019 ) ) ;
#18990 = AXIS2_PLACEMENT_3D ( 'NONE', #12403, #5922, #4558 ) ;
#18991 = ORIENTED_EDGE ( 'NONE', *, *, #2595, .F. ) ;
#18992 = FACE_OUTER_BOUND ( 'NONE', #2832, .T. ) ;
#18993 = CARTESIAN_POINT ( 'NONE',  ( -5.999999999999999112, -7.500000000000047073, 9.999999999999998224 ) ) ;
#18994 =( BOUNDED_SURFACE ( )  B_SPLINE_SURFACE ( 3, 2, ( 
 ( #8790, #18413, #12124, #3866, #12325, #15158, #834, #20293, #4177, #5855, #10352, #4075, #10661, #18300, #7319, #18516, #19981, #16929, #12225, #5642, #13680, #2601, #15256, #9095, #15362, #1150, #5950, #2289, #933, #16726, #2399, #7217, #1045, #7429, #18615, #6064, #7737, #18928, #3026, #7834, #6478, #1250, #1354, #7625, #14295, #12629, #4689, #18721, #1455, #10875, #12432, #6369, #17450, #15567, #4585, #13992, #20603, #9597, #19142, #20706, #19033, #14408, #6255, #11176, #18827, #4390, #1657, #12739, #9502, #2918, #10771, #15875, #14196, #17549, #9403, #20509, #15670, #9192, #10973, #17343, #14100, #17140, #2819, #11079, #3129, #1550, #3226, #7928, #20401, #6163, #15975, #4489, #4795, #17239, #8042 ),
 ( #92, #9295, #12530, #15775, #14722, #3535, #4024, #16669, #11963, #19449, #18361, #7170, #9911, #19935, #11271, #5204, #17766, #14513, #288, #19242, #6573, #785, #190, #5106, #1763, #17962, #9812, #11582, #13533, #11486, #6679, #12937, #16198, #16292, #8245, #19342, #5593, #13048, #4997, #8150, #400, #1964, #10408, #16780, #17865, #3434, #11376, #8346, #1863, #6782, #13152, #19549, #3917, #2448, #17652, #14611, #10298, #2346, #3325, #8841, #8739, #15108, #15208, #884, #12838, #4891, #9707, #16094, #18877, #15725, #2657, #2768, #7577, #12485, #8936, #9047, #7377, #12383, #17288, #1201, #15615, #4443, #15416, #1100, #2970, #7479, #13740, #20457, #13840, #20143, #16879, #15516, #17091, #1298, #7679 ),
 ( #12273, #2549, #9147, #13940, #20342, #20243, #6114, #12074, #15307, #5803, #5901, #18465, #4538, #12174, #2868, #4334, #18562, #6006, #18665, #10718, #4227, #10923, #7269, #18776, #10826, #17191, #9346, #988, #9245, #10607, #14048, #10508, #16980, #13630, #20038, #5702, #4127, #14354, #14463, #6529, #14565, #12789, #1406, #19087, #11434, #12684, #6426, #15925, #9653, #7788, #1602, #7981, #6627, #1813, #15826, #19192, #3178, #19398, #14151, #11326, #20653, #9552, #12579, #8199, #5057, #238, #17398, #12996, #17498, #17713, #11028, #40, #143, #20558, #4845, #6209, #3485, #11226, #1715, #18980, #17602, #12890, #19294, #1503, #9763, #3275, #16039, #17818, #4947, #9861, #8100, #4635, #16148, #3384, #3080 ),
 ( #9454, #7885, #14244, #6310, #4742, #11129, #2120, #5155, #650, #13199, #14972, #16639, #14873, #10073, #16343, #19598, #19697, #5251, #8707, #11534, #5360, #14669, #18130, #8502, #16245, #19912, #17913, #349, #3996, #13101, #6929, #18229, #451, #11628, #2218, #6736, #1914, #5466, #9961, #3580, #761, #18018, #6830, #3689, #11738, #8295, #19503, #16447, #549, #11937, #16542, #11838, #2018, #13296, #2319, #8408, #3795, #10172, #8601, #7038, #3891, #13407, #19812, #10271, #15079, #7146, #13510, #5566, #18333, #14775, #10585, #10485, #18440, #16855, #12249, #2844, #18540, #4102, #20117, #16953, #15390, #20218, #18854, #13606, #13711, #20010, #5981, #4307, #17063, #10381, #13816, #2522, #8914, #18750, #9123 ),
 ( #10692, #15590, #12045, #5780, #15282, #15491, #5674, #960, #4416, #7553, #20433, #16754, #2632, #2743, #1175, #9220, #1075, #2425, #7349, #6092, #12149, #7454, #4203, #18641, #8816, #9019, #5879, #1274, #10800, #13916, #20318, #12356, #7654, #15184, #17169, #14024, #12460, #861, #7244, #1787, #11298, #20533, #9735, #20629, #119, #14128, #11106, #4823, #10899, #14326, #3251, #17577, #18952, #12866, #6399, #15899, #16120, #8072, #3356, #17477, #8174, #19268, #1578, #17685, #2941, #9623, #9430, #6186, #12656, #17262, #4607, #4920, #12554, #3155, #11001, #16009, #1479, #1686, #14542, #9527, #19059, #17370, #7859, #7953, #6282, #3056, #214, #4717, #15802, #14221, #12766, #11, #6600, #12967, #19169 ),
 ( #11204, #14437, #6504, #4515, #9323, #15698, #1382, #7763, #17891, #17991, #3458, #18206, #19478, #14946, #16420, #5131, #5336, #10046, #3661, #9938, #10246, #7122, #14750, #14848, #19671, #3868, #322, #428, #11510, #3770, #1890, #16317, #7015, #16520, #8685, #19371, #11606, #11709, #10149, #11813, #2097, #5026, #1993, #15056, #8378, #8480, #13175, #6903, #11406, #19574, #5228, #16613, #19784, #13076, #524, #6807, #2293, #17792, #8577, #3558, #13271, #9836, #5444, #738, #16223, #14640, #8270, #18106, #626, #6707, #2194, #13382, #11913, #18520, #5543, #15570, #16932, #12329, #13794, #1254, #2497, #5954, #2403, #2604, #18304, #15366, #20094, #13486, #17146, #8794, #3969, #19887, #10356, #4180, #15471 ),
 ( #16730, #15161, #2718, #7220, #837, #18726, #8893, #18416, #937, #8994, #13583, #19984, #4078, #10466, #9196, #20198, #9099, #5647, #7323, #20296, #12020, #1050, #7432, #15259, #5859, #1153, #13685, #12228, #18618, #5757, #4393, #4280, #10776, #16833, #12128, #10563, #10666, #17040, #7530, #13896, #2823, #15780, #15675, #17349, #7838, #12633, #17454, #16098, #10879, #10977, #17242, #3230, #1555, #14299, #7628, #11083, #20513, #1359, #15980, #6375, #4494, #14200, #2922, #97, #13998, #6166, #4799, #20609, #6260, #9300, #7742, #7933, #1661, #11180, #3031, #1459, #17656, #9506, #19246, #8049, #9601, #20711, #3330, #15878, #6482, #14105, #20406, #11276, #14412, #19145, #12534, #6068, #17555, #3132, #12842 ) ),
 .UNSPECIFIED., .T., .F., .F. ) 
 B_SPLINE_SURFACE_WITH_KNOTS ( ( 4, 3, 4 ),
 ( 3, 2, 2, 2, 2, 2, 2, 2, 2, 2, 2, 2, 2, 2, 2, 2, 2, 2, 2, 2, 2, 2, 2, 2, 2, 2, 2, 2, 2, 2, 2, 2, 2, 2, 2, 2, 2, 2, 2, 2, 2, 2, 2, 2, 2, 2, 2, 3 ),
 ( 0.000000000000000000, 0.5000000000000000000, 1.000000000000000000 ),
 ( 0.000000000000000000, 0.02083333333333333218, 0.04166666666666666435, 0.06250000000000000000, 0.08333333333333332871, 0.1041666666666666713, 0.1250000000000000000, 0.1458333333333333426, 0.1666666666666666574, 0.1875000000000000000, 0.2083333333333333426, 0.2291666666666666574, 0.2500000000000000000, 0.2708333333333333148, 0.2916666666666666852, 0.3125000000000000000, 0.3333333333333333148, 0.3541666666666666852, 0.3750000000000000000, 0.3958333333333333148, 0.4166666666666666852, 0.4375000000000000000, 0.4583333333333333148, 0.4791666666666666852, 0.5000000000000000000, 0.5208333333333333703, 0.5416666666666666297, 0.5625000000000000000, 0.5833333333333333703, 0.6041666666666666297, 0.6250000000000000000, 0.6458333333333333703, 0.6666666666666666297, 0.6875000000000000000, 0.7083333333333333703, 0.7291666666666666297, 0.7500000000000000000, 0.7708333333333333703, 0.7916666666666666297, 0.8125000000000000000, 0.8333333333333333703, 0.8541666666666666297, 0.8750000000000000000, 0.8958333333333333703, 0.9166666666666666297, 0.9375000000000000000, 0.9583333333333333703, 0.9650437087885355147 ),
 .UNSPECIFIED. ) 
 GEOMETRIC_REPRESENTATION_ITEM ( )  RATIONAL_B_SPLINE_SURFACE ( (
 ( 1.000000000000000000, 0.9238795325112867385, 1.000000000000000000, 0.9238795325112867385, 1.000000000000000000, 0.9238795325112867385, 1.000000000000000000, 0.9238795325112867385, 1.000000000000000000, 0.9238795325112867385, 1.000000000000000000, 0.9238795325112867385, 1.000000000000000000, 0.9238795325112867385, 1.000000000000000000, 0.9238795325112867385, 1.000000000000000000, 0.9238795325112867385, 1.000000000000000000, 0.9238795325112867385, 1.000000000000000000, 0.9238795325112867385, 1.000000000000000000, 0.9238795325112867385, 1.000000000000000000, 0.9238795325112867385, 1.000000000000000000, 0.9238795325112867385, 1.000000000000000000, 0.9238795325112867385, 1.000000000000000000, 0.9238795325112867385, 1.000000000000000000, 0.9238795325112867385, 1.000000000000000000, 0.9238795325112867385, 1.000000000000000000, 0.9238795325112867385, 1.000000000000000000, 0.9238795325112867385, 1.000000000000000000, 0.9238795325112867385, 1.000000000000000000, 0.9238795325112867385, 1.000000000000000000, 0.9238795325112867385, 1.000000000000000000, 0.9238795325112867385, 1.000000000000000000, 0.9238795325112867385, 1.000000000000000000, 0.9238795325112867385, 1.000000000000000000, 0.9238795325112867385, 1.000000000000000000, 0.9238795325112867385, 1.000000000000000000, 0.9238795325112867385, 1.000000000000000000, 0.9238795325112867385, 1.000000000000000000, 0.9238795325112867385, 1.000000000000000000, 0.9238795325112867385, 1.000000000000000000, 0.9238795325112867385, 1.000000000000000000, 0.9238795325112867385, 1.000000000000000000, 0.9238795325112867385, 1.000000000000000000, 0.9238795325112867385, 1.000000000000000000, 0.9238795325112867385, 1.000000000000000000, 0.9238795325112867385, 1.000000000000000000, 0.9238795325112867385, 1.000000000000000000, 0.9238795325112867385, 1.000000000000000000, 0.9238795325112867385, 1.000000000000000000, 0.9238795325112867385, 1.000000000000000000, 0.9238795325112867385, 1.000000000000000000, 0.9238795325112867385, 1.000000000000000000, 0.9238795325112867385, 1.000000000000000000, 0.9238795325112867385, 1.000000000000000000, 0.9754817479996107377, 0.9667580569362973497),
 ( 0.3333333333333333703, 0.3079598441704289313, 0.3333333333333333703, 0.3079598441704289313, 0.3333333333333333703, 0.3079598441704289313, 0.3333333333333333703, 0.3079598441704289313, 0.3333333333333333703, 0.3079598441704289313, 0.3333333333333333703, 0.3079598441704289313, 0.3333333333333333703, 0.3079598441704289313, 0.3333333333333333703, 0.3079598441704289313, 0.3333333333333333703, 0.3079598441704289313, 0.3333333333333333703, 0.3079598441704289313, 0.3333333333333333703, 0.3079598441704289313, 0.3333333333333333703, 0.3079598441704289313, 0.3333333333333333703, 0.3079598441704289313, 0.3333333333333333703, 0.3079598441704289313, 0.3333333333333333703, 0.3079598441704289313, 0.3333333333333333703, 0.3079598441704289313, 0.3333333333333333703, 0.3079598441704289313, 0.3333333333333333703, 0.3079598441704289313, 0.3333333333333333703, 0.3079598441704289313, 0.3333333333333333703, 0.3079598441704289313, 0.3333333333333333703, 0.3079598441704289313, 0.3333333333333333703, 0.3079598441704289313, 0.3333333333333333703, 0.3079598441704289313, 0.3333333333333333703, 0.3079598441704289313, 0.3333333333333333703, 0.3079598441704289313, 0.3333333333333333703, 0.3079598441704289313, 0.3333333333333333703, 0.3079598441704289313, 0.3333333333333333703, 0.3079598441704289313, 0.3333333333333333703, 0.3079598441704289313, 0.3333333333333333703, 0.3079598441704289313, 0.3333333333333333703, 0.3079598441704289313, 0.3333333333333333703, 0.3079598441704289313, 0.3333333333333333703, 0.3079598441704289313, 0.3333333333333333703, 0.3079598441704289313, 0.3333333333333333703, 0.3079598441704289313, 0.3333333333333333703, 0.3079598441704289313, 0.3333333333333333703, 0.3079598441704289313, 0.3333333333333333703, 0.3079598441704289313, 0.3333333333333333703, 0.3079598441704289313, 0.3333333333333333703, 0.3079598441704289313, 0.3333333333333333703, 0.3079598441704289313, 0.3333333333333333703, 0.3079598441704289313, 0.3333333333333333703, 0.3079598441704289313, 0.3333333333333333703, 0.3079598441704289313, 0.3333333333333333703, 0.3079598441704289313, 0.3333333333333333703, 0.3079598441704289313, 0.3333333333333333703, 0.3251605826665369681, 0.3222526856454325239),
 ( 0.3333333333333333703, 0.3079598441704289313, 0.3333333333333333703, 0.3079598441704289313, 0.3333333333333333703, 0.3079598441704289313, 0.3333333333333333703, 0.3079598441704289313, 0.3333333333333333703, 0.3079598441704289313, 0.3333333333333333703, 0.3079598441704289313, 0.3333333333333333703, 0.3079598441704289313, 0.3333333333333333703, 0.3079598441704289313, 0.3333333333333333703, 0.3079598441704289313, 0.3333333333333333703, 0.3079598441704289313, 0.3333333333333333703, 0.3079598441704289313, 0.3333333333333333703, 0.3079598441704289313, 0.3333333333333333703, 0.3079598441704289313, 0.3333333333333333703, 0.3079598441704289313, 0.3333333333333333703, 0.3079598441704289313, 0.3333333333333333703, 0.3079598441704289313, 0.3333333333333333703, 0.3079598441704289313, 0.3333333333333333703, 0.3079598441704289313, 0.3333333333333333703, 0.3079598441704289313, 0.3333333333333333703, 0.3079598441704289313, 0.3333333333333333703, 0.3079598441704289313, 0.3333333333333333703, 0.3079598441704289313, 0.3333333333333333703, 0.3079598441704289313, 0.3333333333333333703, 0.3079598441704289313, 0.3333333333333333703, 0.3079598441704289313, 0.3333333333333333703, 0.3079598441704289313, 0.3333333333333333703, 0.3079598441704289313, 0.3333333333333333703, 0.3079598441704289313, 0.3333333333333333703, 0.3079598441704289313, 0.3333333333333333703, 0.3079598441704289313, 0.3333333333333333703, 0.3079598441704289313, 0.3333333333333333703, 0.3079598441704289313, 0.3333333333333333703, 0.3079598441704289313, 0.3333333333333333703, 0.3079598441704289313, 0.3333333333333333703, 0.3079598441704289313, 0.3333333333333333703, 0.3079598441704289313, 0.3333333333333333703, 0.3079598441704289313, 0.3333333333333333703, 0.3079598441704289313, 0.3333333333333333703, 0.3079598441704289313, 0.3333333333333333703, 0.3079598441704289313, 0.3333333333333333703, 0.3079598441704289313, 0.3333333333333333703, 0.3079598441704289313, 0.3333333333333333703, 0.3079598441704289313, 0.3333333333333333703, 0.3079598441704289313, 0.3333333333333333703, 0.3079598441704289313, 0.3333333333333333703, 0.3079598441704289313, 0.3333333333333333703, 0.3251605826665369681, 0.3222526856454325239),
 ( 1.000000000000000000, 0.9238795325112867385, 1.000000000000000000, 0.9238795325112867385, 1.000000000000000000, 0.9238795325112867385, 1.000000000000000000, 0.9238795325112867385, 1.000000000000000000, 0.9238795325112867385, 1.000000000000000000, 0.9238795325112867385, 1.000000000000000000, 0.9238795325112867385, 1.000000000000000000, 0.9238795325112867385, 1.000000000000000000, 0.9238795325112867385, 1.000000000000000000, 0.9238795325112867385, 1.000000000000000000, 0.9238795325112867385, 1.000000000000000000, 0.9238795325112867385, 1.000000000000000000, 0.9238795325112867385, 1.000000000000000000, 0.9238795325112867385, 1.000000000000000000, 0.9238795325112867385, 1.000000000000000000, 0.9238795325112867385, 1.000000000000000000, 0.9238795325112867385, 1.000000000000000000, 0.9238795325112867385, 1.000000000000000000, 0.9238795325112867385, 1.000000000000000000, 0.9238795325112867385, 1.000000000000000000, 0.9238795325112867385, 1.000000000000000000, 0.9238795325112867385, 1.000000000000000000, 0.9238795325112867385, 1.000000000000000000, 0.9238795325112867385, 1.000000000000000000, 0.9238795325112867385, 1.000000000000000000, 0.9238795325112867385, 1.000000000000000000, 0.9238795325112867385, 1.000000000000000000, 0.9238795325112867385, 1.000000000000000000, 0.9238795325112867385, 1.000000000000000000, 0.9238795325112867385, 1.000000000000000000, 0.9238795325112867385, 1.000000000000000000, 0.9238795325112867385, 1.000000000000000000, 0.9238795325112867385, 1.000000000000000000, 0.9238795325112867385, 1.000000000000000000, 0.9238795325112867385, 1.000000000000000000, 0.9238795325112867385, 1.000000000000000000, 0.9238795325112867385, 1.000000000000000000, 0.9238795325112867385, 1.000000000000000000, 0.9238795325112867385, 1.000000000000000000, 0.9238795325112867385, 1.000000000000000000, 0.9238795325112867385, 1.000000000000000000, 0.9238795325112867385, 1.000000000000000000, 0.9238795325112867385, 1.000000000000000000, 0.9238795325112867385, 1.000000000000000000, 0.9238795325112867385, 1.000000000000000000, 0.9238795325112867385, 1.000000000000000000, 0.9754817479996107377, 0.9667580569362973497),
 ( 0.3333333333333333703, 0.3079598441704289313, 0.3333333333333333703, 0.3079598441704289313, 0.3333333333333333703, 0.3079598441704289313, 0.3333333333333333703, 0.3079598441704289313, 0.3333333333333333703, 0.3079598441704289313, 0.3333333333333333703, 0.3079598441704289313, 0.3333333333333333703, 0.3079598441704289313, 0.3333333333333333703, 0.3079598441704289313, 0.3333333333333333703, 0.3079598441704289313, 0.3333333333333333703, 0.3079598441704289313, 0.3333333333333333703, 0.3079598441704289313, 0.3333333333333333703, 0.3079598441704289313, 0.3333333333333333703, 0.3079598441704289313, 0.3333333333333333703, 0.3079598441704289313, 0.3333333333333333703, 0.3079598441704289313, 0.3333333333333333703, 0.3079598441704289313, 0.3333333333333333703, 0.3079598441704289313, 0.3333333333333333703, 0.3079598441704289313, 0.3333333333333333703, 0.3079598441704289313, 0.3333333333333333703, 0.3079598441704289313, 0.3333333333333333703, 0.3079598441704289313, 0.3333333333333333703, 0.3079598441704289313, 0.3333333333333333703, 0.3079598441704289313, 0.3333333333333333703, 0.3079598441704289313, 0.3333333333333333703, 0.3079598441704289313, 0.3333333333333333703, 0.3079598441704289313, 0.3333333333333333703, 0.3079598441704289313, 0.3333333333333333703, 0.3079598441704289313, 0.3333333333333333703, 0.3079598441704289313, 0.3333333333333333703, 0.3079598441704289313, 0.3333333333333333703, 0.3079598441704289313, 0.3333333333333333703, 0.3079598441704289313, 0.3333333333333333703, 0.3079598441704289313, 0.3333333333333333703, 0.3079598441704289313, 0.3333333333333333703, 0.3079598441704289313, 0.3333333333333333703, 0.3079598441704289313, 0.3333333333333333703, 0.3079598441704289313, 0.3333333333333333703, 0.3079598441704289313, 0.3333333333333333703, 0.3079598441704289313, 0.3333333333333333703, 0.3079598441704289313, 0.3333333333333333703, 0.3079598441704289313, 0.3333333333333333703, 0.3079598441704289313, 0.3333333333333333703, 0.3079598441704289313, 0.3333333333333333703, 0.3079598441704289313, 0.3333333333333333703, 0.3079598441704289313, 0.3333333333333333703, 0.3079598441704289313, 0.3333333333333333703, 0.3251605826665369681, 0.3222526856454325239),
 ( 0.3333333333333333703, 0.3079598441704289313, 0.3333333333333333703, 0.3079598441704289313, 0.3333333333333333703, 0.3079598441704289313, 0.3333333333333333703, 0.3079598441704289313, 0.3333333333333333703, 0.3079598441704289313, 0.3333333333333333703, 0.3079598441704289313, 0.3333333333333333703, 0.3079598441704289313, 0.3333333333333333703, 0.3079598441704289313, 0.3333333333333333703, 0.3079598441704289313, 0.3333333333333333703, 0.3079598441704289313, 0.3333333333333333703, 0.3079598441704289313, 0.3333333333333333703, 0.3079598441704289313, 0.3333333333333333703, 0.3079598441704289313, 0.3333333333333333703, 0.3079598441704289313, 0.3333333333333333703, 0.3079598441704289313, 0.3333333333333333703, 0.3079598441704289313, 0.3333333333333333703, 0.3079598441704289313, 0.3333333333333333703, 0.3079598441704289313, 0.3333333333333333703, 0.3079598441704289313, 0.3333333333333333703, 0.3079598441704289313, 0.3333333333333333703, 0.3079598441704289313, 0.3333333333333333703, 0.3079598441704289313, 0.3333333333333333703, 0.3079598441704289313, 0.3333333333333333703, 0.3079598441704289313, 0.3333333333333333703, 0.3079598441704289313, 0.3333333333333333703, 0.3079598441704289313, 0.3333333333333333703, 0.3079598441704289313, 0.3333333333333333703, 0.3079598441704289313, 0.3333333333333333703, 0.3079598441704289313, 0.3333333333333333703, 0.3079598441704289313, 0.3333333333333333703, 0.3079598441704289313, 0.3333333333333333703, 0.3079598441704289313, 0.3333333333333333703, 0.3079598441704289313, 0.3333333333333333703, 0.3079598441704289313, 0.3333333333333333703, 0.3079598441704289313, 0.3333333333333333703, 0.3079598441704289313, 0.3333333333333333703, 0.3079598441704289313, 0.3333333333333333703, 0.3079598441704289313, 0.3333333333333333703, 0.3079598441704289313, 0.3333333333333333703, 0.3079598441704289313, 0.3333333333333333703, 0.3079598441704289313, 0.3333333333333333703, 0.3079598441704289313, 0.3333333333333333703, 0.3079598441704289313, 0.3333333333333333703, 0.3079598441704289313, 0.3333333333333333703, 0.3079598441704289313, 0.3333333333333333703, 0.3079598441704289313, 0.3333333333333333703, 0.3251605826665369681, 0.3222526856454325239),
 ( 1.000000000000000000, 0.9238795325112867385, 1.000000000000000000, 0.9238795325112867385, 1.000000000000000000, 0.9238795325112867385, 1.000000000000000000, 0.9238795325112867385, 1.000000000000000000, 0.9238795325112867385, 1.000000000000000000, 0.9238795325112867385, 1.000000000000000000, 0.9238795325112867385, 1.000000000000000000, 0.9238795325112867385, 1.000000000000000000, 0.9238795325112867385, 1.000000000000000000, 0.9238795325112867385, 1.000000000000000000, 0.9238795325112867385, 1.000000000000000000, 0.9238795325112867385, 1.000000000000000000, 0.9238795325112867385, 1.000000000000000000, 0.9238795325112867385, 1.000000000000000000, 0.9238795325112867385, 1.000000000000000000, 0.9238795325112867385, 1.000000000000000000, 0.9238795325112867385, 1.000000000000000000, 0.9238795325112867385, 1.000000000000000000, 0.9238795325112867385, 1.000000000000000000, 0.9238795325112867385, 1.000000000000000000, 0.9238795325112867385, 1.000000000000000000, 0.9238795325112867385, 1.000000000000000000, 0.9238795325112867385, 1.000000000000000000, 0.9238795325112867385, 1.000000000000000000, 0.9238795325112867385, 1.000000000000000000, 0.9238795325112867385, 1.000000000000000000, 0.9238795325112867385, 1.000000000000000000, 0.9238795325112867385, 1.000000000000000000, 0.9238795325112867385, 1.000000000000000000, 0.9238795325112867385, 1.000000000000000000, 0.9238795325112867385, 1.000000000000000000, 0.9238795325112867385, 1.000000000000000000, 0.9238795325112867385, 1.000000000000000000, 0.9238795325112867385, 1.000000000000000000, 0.9238795325112867385, 1.000000000000000000, 0.9238795325112867385, 1.000000000000000000, 0.9238795325112867385, 1.000000000000000000, 0.9238795325112867385, 1.000000000000000000, 0.9238795325112867385, 1.000000000000000000, 0.9238795325112867385, 1.000000000000000000, 0.9238795325112867385, 1.000000000000000000, 0.9238795325112867385, 1.000000000000000000, 0.9238795325112867385, 1.000000000000000000, 0.9238795325112867385, 1.000000000000000000, 0.9238795325112867385, 1.000000000000000000, 0.9238795325112867385, 1.000000000000000000, 0.9754817479996107377, 0.9667580569362973497) ) ) 
 REPRESENTATION_ITEM ( '' )  SURFACE ( )  );
#18995 = CARTESIAN_POINT ( 'NONE',  ( 13.87490072368896676, 4.990068513505961256, 3.999999999999998224 ) ) ;
#18996 = CARTESIAN_POINT ( 'NONE',  ( 1.407845757905374695, -8.364917468222230923, 1.622643865078341907 ) ) ;
#18997 = CARTESIAN_POINT ( 'NONE',  ( 14.49999999999998579, -21.99999999999999645, 11.68378559369222280 ) ) ;
#18998 = DIRECTION ( 'NONE',  ( -1.000000000000000000, 0.000000000000000000, 0.000000000000000000 ) ) ;
#18999 = EDGE_CURVE ( 'NONE', #2052, #5735, #15172, .T. ) ;
#19000 = PLANE ( 'NONE',  #8306 ) ;
#19001 = CARTESIAN_POINT ( 'NONE',  ( 15.00000000000000000, 0.000000000000000000, 1.000000000000000000 ) ) ;
#19002 = EDGE_CURVE ( 'NONE', #16377, #9583, #10159, .T. ) ;
#19003 = CARTESIAN_POINT ( 'NONE',  ( -2.645259258103298983, -10.28229522185712241, 2.672449792925449596 ) ) ;
#19004 = AXIS2_PLACEMENT_3D ( 'NONE', #15660, #6470, #4783 ) ;
#19005 = CARTESIAN_POINT ( 'NONE',  ( 13.27780858231679417, -21.02099543870833998, 3.035098964749253003 ) ) ;
#19006 = CARTESIAN_POINT ( 'NONE',  ( -12.62500000000002132, -19.50000000000273559, 4.083333333315724012 ) ) ;
#19007 = CARTESIAN_POINT ( 'NONE',  ( -12.90280858231679595, -22.46490103525074034, 2.520995438708341307 ) ) ;
#19008 = CARTESIAN_POINT ( 'NONE',  ( -7.284691417683176518, -24.52099543870834708, 4.484846433055073689 ) ) ;
#19009 = VECTOR ( 'NONE', #5077, 1000.000000000000000 ) ;
#19010 = ADVANCED_FACE ( 'NONE', ( #14957 ), #2413, .T. ) ;
#19011 = ORIENTED_EDGE ( 'NONE', *, *, #4317, .T. ) ;
#19012 = CARTESIAN_POINT ( 'NONE',  ( 13.37499999999998401, -19.49999999999998934, 2.439580858552613751 ) ) ;
#19013 = DIRECTION ( 'NONE',  ( 0.000000000000000000, 0.000000000000000000, -1.000000000000000000 ) ) ;
#19014 = EDGE_LOOP ( 'NONE', ( #5514, #1896, #5621, #15906, #6866, #6881, #2806, #4978, #17449, #17495, #16570, #3033, #10389, #18623, #9199, #15597, #8026, #18027, #9690, #4029, #18708, #11559, #8235, #15700, #16291, #12015, #11790, #14571, #7532, #13871, #16875, #9940, #5832, #15312, #20145, #1208, #10517, #12387, #16501, #19373, #7990, #19737, #13110, #19222, #8667, #10874, #17460, #5028, #14953, #15658, #5983, #892, #15755, #5161, #744, #20194, #16548, #7814, #3002, #13836, #20400, #557, #17238, #15449, #11763, #6221, #10469, #3112, #11740, #17748, #19869, #9486, #9002, #652, #8887, #16609, #20494, #17609, #3137, #16615, #12130, #13206, #10840, #19017, #18662, #3210, #9580, #7533, #1717, #3998, #14363, #8872, #1934, #5915, #6536, #5986, #5525, #6539, #15290, #7635, #8274, #15446, #19833, #325, #17820, #10133, #9178, #781, #11714, #8125, #10782, #6042, #156, #358, #17148, #15146, #8153, #8634, #19149, #14298 ) ) ;
#19015 = CIRCLE ( 'NONE', #9973, 0.3749999999999997224 ) ;
#19016 = LINE ( 'NONE', #3111, #5969 ) ;
#19017 = ORIENTED_EDGE ( 'NONE', *, *, #8465, .T. ) ;
#19018 = CARTESIAN_POINT ( 'NONE',  ( 3.277163086644854229, -14.76879761173520578, 3.824673233536266537 ) ) ;
#19019 = EDGE_CURVE ( 'NONE', #19533, #5029, #13187, .T. ) ;
#19020 = CIRCLE ( 'NONE', #3295, 0.2500000000000002220 ) ;
#19021 = VERTEX_POINT ( 'NONE', #2106 ) ;
#19022 = CARTESIAN_POINT ( 'NONE',  ( 10.75344141768317741, -21.94931252712233061, 1.749999999999998446 ) ) ;
#19023 = CARTESIAN_POINT ( 'NONE',  ( 15.00000000000000355, -5.999999999999996447, 2.000000000000000000 ) ) ;
#19024 = VECTOR ( 'NONE', #1255, 1000.000000000000000 ) ;
#19025 = CARTESIAN_POINT ( 'NONE',  ( -1.797604806073912709, -9.120796646272857799, 2.374153755450133740 ) ) ;
#19026 = LINE ( 'NONE', #4483, #14315 ) ;
#19027 = CARTESIAN_POINT ( 'NONE',  ( -10.27780858231679417, -20.27099543870833642, 2.724438792969431589 ) ) ;
#19028 = DIRECTION ( 'NONE',  ( 4.625929269271486900E-15, 1.000000000000000000, 0.000000000000000000 ) ) ;
#19029 = CARTESIAN_POINT ( 'NONE',  ( 4.378441417683176518, -24.50000000000000000, 3.449312527122335048 ) ) ;
#19030 = CARTESIAN_POINT ( 'NONE',  ( -9.805650798910056309, 4.999999999999999112, 0.000000000000000000 ) ) ;
#19031 = CARTESIAN_POINT ( 'NONE',  ( -8.690941417683177406, -23.27327832286946219, 4.701595411283453707 ) ) ;
#19032 = ORIENTED_EDGE ( 'NONE', *, *, #9784, .T. ) ;
#19033 = CARTESIAN_POINT ( 'NONE',  ( 7.746558582316794173, -21.94931252712234482, 5.250000000000000888 ) ) ;
#19034 = VECTOR ( 'NONE', #14816, 1000.000000000000000 ) ;
#19035 = DIRECTION ( 'NONE',  ( -1.000000000000000000, 0.000000000000000000, 0.000000000000000000 ) ) ;
#19036 = CARTESIAN_POINT ( 'NONE',  ( -12.66383876651304874, -19.03864229108970463, 6.262079579155994224 ) ) ;
#19037 = AXIS2_PLACEMENT_3D ( 'NONE', #14260, #3094, #1421 ) ;
#19038 = LINE ( 'NONE', #4695, #6626 ) ;
#19039 = CARTESIAN_POINT ( 'NONE',  ( 3.499999999999998668, -19.50000000000000000, 1.000000000000000000 ) ) ;
#19040 = VECTOR ( 'NONE', #20072, 1000.000000000000000 ) ;
#19041 = EDGE_LOOP ( 'NONE', ( #9558, #2561, #11233, #1534 ) ) ;
#19042 = VECTOR ( 'NONE', #1327, 1000.000000000000000 ) ;
#19043 = DIRECTION ( 'NONE',  ( 0.000000000000000000, 1.000000000000000000, -0.000000000000000000 ) ) ;
#19044 = ORIENTED_EDGE ( 'NONE', *, *, #356, .F. ) ;
#19045 = EDGE_CURVE ( 'NONE', #8332, #3444, #19682, .T. ) ;
#19046 = DIRECTION ( 'NONE',  ( 1.000000000000000000, 0.000000000000000000, 0.000000000000000000 ) ) ;
#19047 = ORIENTED_EDGE ( 'NONE', *, *, #10755, .T. ) ;
#19048 = CARTESIAN_POINT ( 'NONE',  ( -13.27780858231679417, -19.52099543870833642, 2.413778621189609286 ) ) ;
#19049 = DIRECTION ( 'NONE',  ( 0.000000000000000000, 0.000000000000000000, 1.000000000000000000 ) ) ;
#19050 = DIRECTION ( 'NONE',  ( 0.000000000000000000, 0.000000000000000000, 1.000000000000000000 ) ) ;
#19051 = CARTESIAN_POINT ( 'NONE',  ( 2.088806020750596737, -10.42712783963456857, 1.767030719737609168 ) ) ;
#19052 =( GEOMETRIC_REPRESENTATION_CONTEXT ( 3 ) GLOBAL_UNCERTAINTY_ASSIGNED_CONTEXT ( ( #1081 ) ) GLOBAL_UNIT_ASSIGNED_CONTEXT ( ( #17353, #15681, #18936 ) ) REPRESENTATION_CONTEXT ( 'NONE', 'WORKASPACE' ) );
#19053 = CARTESIAN_POINT ( 'NONE',  ( 25.54469207716615031, 9.000000000000001776, 1.000000000000000000 ) ) ;
#19054 = CARTESIAN_POINT ( 'NONE',  ( -13.64827103573800571, -5.699812695207630675, 5.034333296717131034 ) ) ;
#19055 = CARTESIAN_POINT ( 'NONE',  ( 10.09030858231679595, -21.32581373872472597, 1.729004561291657582 ) ) ;
#19056 = CARTESIAN_POINT ( 'NONE',  ( -12.66204031416134335, -19.12946413485185104, 6.260126454156002218 ) ) ;
#19057 = CARTESIAN_POINT ( 'NONE',  ( -0.1250000000000001110, 10.00000000000000000, 1.000000000000000000 ) ) ;
#19058 = CARTESIAN_POINT ( 'NONE',  ( 4.717959273841178636, -21.72818306014730183, 5.243595146365860771 ) ) ;
#19059 = CARTESIAN_POINT ( 'NONE',  ( 5.128441417683177406, -20.99999999999999645, 3.550687472877664952 ) ) ;
#19060 = CARTESIAN_POINT ( 'NONE',  ( -6.996558582316793284, -22.05068747287764452, 1.749999999999998446 ) ) ;
#19061 = ORIENTED_EDGE ( 'NONE', *, *, #9798, .T. ) ;
#19062 = CARTESIAN_POINT ( 'NONE',  ( 13.68663801924254741, -3.762280028282741551, 5.075999963380942503 ) ) ;
#19063 = CARTESIAN_POINT ( 'NONE',  ( 0.000000000000000000, -9.114917468222230923, 1.622643865078341019 ) ) ;
#19064 = ORIENTED_EDGE ( 'NONE', *, *, #2699, .T. ) ;
#19065 = AXIS2_PLACEMENT_3D ( 'NONE', #11590, #5006, #9819 ) ;
#19066 = ORIENTED_EDGE ( 'NONE', *, *, #3665, .F. ) ;
#19067 = DIRECTION ( 'NONE',  ( -1.734723475976807094E-15, 1.000000000000000000, 0.000000000000000000 ) ) ;
#19068 = AXIS2_PLACEMENT_3D ( 'NONE', #13508, #20114, #15388 ) ;
#19069 = CIRCLE ( 'NONE', #19726, 10.00000000000000000 ) ;
#19070 = ADVANCED_FACE ( 'NONE', ( #535 ), #11616, .F. ) ;
#19071 = DIRECTION ( 'NONE',  ( 0.000000000000000000, 0.000000000000000000, 1.000000000000000000 ) ) ;
#19072 = CARTESIAN_POINT ( 'NONE',  ( -3.722205087890566144, -11.52065056559861134, 2.433099166587254558 ) ) ;
#19073 = DIRECTION ( 'NONE',  ( 0.000000000000000000, 1.000000000000000000, 0.000000000000000000 ) ) ;
#19074 = PLANE ( 'NONE',  #1718 ) ;
#19075 = CARTESIAN_POINT ( 'NONE',  ( -12.63465172146706728, -19.76258806590802664, 5.372658420469845986 ) ) ;
#19076 = CARTESIAN_POINT ( 'NONE',  ( 11.87155858231679417, -20.24999999999999289, 3.449312527122348371 ) ) ;
#19077 = EDGE_CURVE ( 'NONE', #1633, #16888, #10365, .T. ) ;
#19078 = DIRECTION ( 'NONE',  ( -0.000000000000000000, -0.000000000000000000, -1.000000000000000000 ) ) ;
#19079 = CARTESIAN_POINT ( 'NONE',  ( 13.12860732321105139, 4.432169822159808703, 6.709107302035562270 ) ) ;
#19080 = CARTESIAN_POINT ( 'NONE',  ( -6.434058582316796837, -23.73192549717337130, 5.303608408759367343 ) ) ;
#19081 = CARTESIAN_POINT ( 'NONE',  ( -2.124709647372160060, -10.68204274815009924, 1.832497960681391147 ) ) ;
#19082 = ORIENTED_EDGE ( 'NONE', *, *, #13066, .F. ) ;
#19083 = CARTESIAN_POINT ( 'NONE',  ( -13.87066368810231154, 4.781016249162736820, 5.617237349937618696 ) ) ;
#19084 = VECTOR ( 'NONE', #16674, 1000.000000000000000 ) ;
#19085 = CARTESIAN_POINT ( 'NONE',  ( -11.75209451496117197, 0.000000000000000000, 0.000000000000000000 ) ) ;
#19086 = VECTOR ( 'NONE', #10089, 1000.000000000000000 ) ;
#19087 = CARTESIAN_POINT ( 'NONE',  ( 8.597191417683177406, -23.08622137881040359, 5.979004561291654696 ) ) ;
#19088 = CARTESIAN_POINT ( 'NONE',  ( -5.222191417683177406, -21.02099543870834353, 3.964901035250761208 ) ) ;
#19089 = VERTEX_POINT ( 'NONE', #8694 ) ;
#19090 = VECTOR ( 'NONE', #11929, 1000.000000000000000 ) ;
#19091 = CARTESIAN_POINT ( 'NONE',  ( 13.37500027835944039, -20.99998594284889464, 4.544258551573043370 ) ) ;
#19092 = AXIS2_PLACEMENT_3D ( 'NONE', #11661, #9795, #3517 ) ;
#19093 = CARTESIAN_POINT ( 'NONE',  ( -3.497260319564023057, 9.000000000000001776, 1.000000000000000000 ) ) ;
#19094 = DIRECTION ( 'NONE',  ( -1.000000000000000000, -0.000000000000000000, -0.000000000000000000 ) ) ;
#19095 = VERTEX_POINT ( 'NONE', #2303 ) ;
#19096 = EDGE_LOOP ( 'NONE', ( #3827, #15678, #5280, #16940 ) ) ;
#19097 = CARTESIAN_POINT ( 'NONE',  ( 2.687849085826861995, 16.00000000000000000, 1.000000000000000000 ) ) ;
#19098 = EDGE_CURVE ( 'NONE', #17042, #17247, #13282, .T. ) ;
#19099 = CARTESIAN_POINT ( 'NONE',  ( 2.499999999999998668, -19.50000000000000000, 1.000000000000000000 ) ) ;
#19100 = VECTOR ( 'NONE', #521, 1000.000000000000000 ) ;
#19101 = CARTESIAN_POINT ( 'NONE',  ( 15.36404127825609400, 4.999999999999999112, 1.000000000000000000 ) ) ;
#19102 = CARTESIAN_POINT ( 'NONE',  ( 2.109407804498405703, -9.207748739546751438, 2.396484790045401603 ) ) ;
#19103 = VECTOR ( 'NONE', #6727, 1000.000000000000000 ) ;
#19104 = CARTESIAN_POINT ( 'NONE',  ( 15.36404127825609400, 4.999999999999999112, 1.000000000000000000 ) ) ;
#19105 = CARTESIAN_POINT ( 'NONE',  ( 2.768424032093183662, -10.00067216410020166, 1.850123365707658785 ) ) ;
#19106 = CARTESIAN_POINT ( 'NONE',  ( 0.000000000000000000, 10.00000000000000000, 1.000000000000000000 ) ) ;
#19107 = CARTESIAN_POINT ( 'NONE',  ( 14.31494360078803041, 10.00000000000000000, 1.000000000000000000 ) ) ;
#19108 =( REPRESENTATION_RELATIONSHIP ('NONE','NONE', #1880, #6045 ) REPRESENTATION_RELATIONSHIP_WITH_TRANSFORMATION ( #10228 )SHAPE_REPRESENTATION_RELATIONSHIP( ) );
#19109 = CARTESIAN_POINT ( 'NONE',  ( -9.000000000000000000, -9.999999999999992895, 2.500000000000000000 ) ) ;
#19110 = CARTESIAN_POINT ( 'NONE',  ( -15.11404127825609223, 0.000000000000000000, 0.000000000000000000 ) ) ;
#19111 = CARTESIAN_POINT ( 'NONE',  ( -9.689245429134309973, 10.00000000000000000, 1.000000000000000000 ) ) ;
#19112 = CARTESIAN_POINT ( 'NONE',  ( -1.797604806073912709, -9.120796646272857799, 2.374153755450133740 ) ) ;
#19113 = CARTESIAN_POINT ( 'NONE',  ( 3.944195004867014909, -21.80034658733847053, 4.481176709221804444 ) ) ;
#19114 = CARTESIAN_POINT ( 'NONE',  ( -12.65650603190776025, -18.65894538865861563, 5.520212342915047365 ) ) ;
#19115 = EDGE_CURVE ( 'NONE', #13902, #7075, #4090, .T. ) ;
#19116 = CARTESIAN_POINT ( 'NONE',  ( -12.34030858231679240, -22.67418626127525982, 5.270995438708342640 ) ) ;
#19117 = CARTESIAN_POINT ( 'NONE',  ( -11.59719141768317563, -22.77556120703057729, 5.229004561291655584 ) ) ;
#19118 = ORIENTED_EDGE ( 'NONE', *, *, #415, .F. ) ;
#19119 = CARTESIAN_POINT ( 'NONE',  ( 13.09455366754861139, 4.212460211200554916, 5.160171780694988719 ) ) ;
#19120 = CARTESIAN_POINT ( 'NONE',  ( 19.73630159782011617, 4.999999999999999112, 1.000000000000000000 ) ) ;
#19121 = ORIENTED_EDGE ( 'NONE', *, *, #13827, .T. ) ;
#19122 = VECTOR ( 'NONE', #13075, 1000.000000000000000 ) ;
#19123 = CARTESIAN_POINT ( 'NONE',  ( 3.999999999999999112, -7.500000000000047073, 2.000000000000000000 ) ) ;
#19124 = ORIENTED_EDGE ( 'NONE', *, *, #19639, .T. ) ;
#19125 = CARTESIAN_POINT ( 'NONE',  ( -5.933390479346035029, 0.000000000000000000, 0.000000000000000000 ) ) ;
#19126 = EDGE_CURVE ( 'NONE', #17639, #17561, #2541, .T. ) ;
#19127 =( BOUNDED_CURVE ( )  B_SPLINE_CURVE ( 2, ( #6358, #6244, #7919, #9587, #15963, #9695, #7822, #12727, #4574, #12617, #6563, #1852, #14600, #17329, #11365, #14283, #17640, #19328, #1646, #8028, #19022, #11259, #12926, #20694, #14398, #3314, #79, #9801, #6468, #16185, #275, #1444, #178, #4675, #12828, #11070, #19230, #17754, #4881, #3117, #16082, #8236, #1753, #9492, #18916, #4986, #6666, #10961, #3014, #9391, #15763, #14185, #20593, #3729, #16576, #14813, #2253, #10003, #6969, #17855, #13340, #389, #10209, #19632, #5290, #16281, #16381, #3522, #8640, #1952, #19742, #11875, #2059, #8445, #488, #6867, #8333, #7081, #10312, #11666, #5094, #18266, #18063, #14710, #6772, #13235, #3928, #13445, #13141, #10108, #16484, #16682, #11474, #2156, #8539 ),
 .UNSPECIFIED., .F., .F. ) 
 B_SPLINE_CURVE_WITH_KNOTS ( ( 3, 2, 2, 2, 2, 2, 2, 2, 2, 2, 2, 2, 2, 2, 2, 2, 2, 2, 2, 2, 2, 2, 2, 2, 2, 2, 2, 2, 2, 2, 2, 2, 2, 2, 2, 2, 2, 2, 2, 2, 2, 2, 2, 2, 2, 2, 2, 3 ),
 ( 0.000000000000000000, 0.02083333333333333218, 0.04166666666666666435, 0.06250000000000000000, 0.08333333333333332871, 0.1041666666666666713, 0.1250000000000000000, 0.1458333333333333426, 0.1666666666666666574, 0.1875000000000000000, 0.2083333333333333426, 0.2291666666666666574, 0.2500000000000000000, 0.2708333333333333148, 0.2916666666666666852, 0.3124999999999999445, 0.3333333333333333148, 0.3541666666666666852, 0.3750000000000000000, 0.3958333333333333148, 0.4166666666666666852, 0.4375000000000000555, 0.4583333333333333148, 0.4791666666666666852, 0.5000000000000000000, 0.5208333333333333703, 0.5416666666666666297, 0.5625000000000000000, 0.5833333333333333703, 0.6041666666666666297, 0.6249999999999998890, 0.6458333333333333703, 0.6666666666666666297, 0.6875000000000000000, 0.7083333333333333703, 0.7291666666666666297, 0.7500000000000000000, 0.7708333333333333703, 0.7916666666666666297, 0.8125000000000000000, 0.8333333333333333703, 0.8541666666666666297, 0.8750000000000001110, 0.8958333333333333703, 0.9166666666666666297, 0.9375000000000000000, 0.9583333333333333703, 0.9650437087885355147 ),
 .UNSPECIFIED. ) 
 CURVE ( )  GEOMETRIC_REPRESENTATION_ITEM ( )  RATIONAL_B_SPLINE_CURVE ( ( 1.000000000000000000, 0.9238795325112867385, 1.000000000000000000, 0.9238795325112867385, 1.000000000000000000, 0.9238795325112867385, 1.000000000000000000, 0.9238795325112867385, 1.000000000000000000, 0.9238795325112867385, 1.000000000000000000, 0.9238795325112867385, 1.000000000000000000, 0.9238795325112867385, 1.000000000000000000, 0.9238795325112867385, 1.000000000000000000, 0.9238795325112867385, 1.000000000000000000, 0.9238795325112867385, 1.000000000000000000, 0.9238795325112867385, 1.000000000000000000, 0.9238795325112867385, 1.000000000000000000, 0.9238795325112867385, 1.000000000000000000, 0.9238795325112867385, 1.000000000000000000, 0.9238795325112867385, 1.000000000000000000, 0.9238795325112867385, 1.000000000000000000, 0.9238795325112867385, 1.000000000000000000, 0.9238795325112867385, 1.000000000000000000, 0.9238795325112867385, 1.000000000000000000, 0.9238795325112867385, 1.000000000000000000, 0.9238795325112867385, 1.000000000000000000, 0.9238795325112867385, 1.000000000000000000, 0.9238795325112867385, 1.000000000000000000, 0.9238795325112867385, 1.000000000000000000, 0.9238795325112867385, 1.000000000000000000, 0.9238795325112867385, 1.000000000000000000, 0.9238795325112867385, 1.000000000000000000, 0.9238795325112867385, 1.000000000000000000, 0.9238795325112867385, 1.000000000000000000, 0.9238795325112867385, 1.000000000000000000, 0.9238795325112867385, 1.000000000000000000, 0.9238795325112867385, 1.000000000000000000, 0.9238795325112867385, 1.000000000000000000, 0.9238795325112867385, 1.000000000000000000, 0.9238795325112867385, 1.000000000000000000, 0.9238795325112867385, 1.000000000000000000, 0.9238795325112867385, 1.000000000000000000, 0.9238795325112867385, 1.000000000000000000, 0.9238795325112867385, 1.000000000000000000, 0.9238795325112867385, 1.000000000000000000, 0.9238795325112867385, 1.000000000000000000, 0.9238795325112867385, 1.000000000000000000, 0.9238795325112867385, 1.000000000000000000, 0.9238795325112867385, 1.000000000000000000, 0.9238795325112867385, 1.000000000000000000, 0.9238795325112867385, 1.000000000000000000, 0.9754817479996107377, 0.9667580569362973497 ) ) 
 REPRESENTATION_ITEM ( '' )  );
#19128 = EDGE_CURVE ( 'NONE', #10227, #1283, #8588, .T. ) ;
#19129 = VERTEX_POINT ( 'NONE', #7230 ) ;
#19130 = CARTESIAN_POINT ( 'NONE',  ( 13.12500000000000178, 5.000000000000047962, 2.000000000000000000 ) ) ;
#19131 = DIRECTION ( 'NONE',  ( 1.000000000000000000, 0.000000000000000000, 0.000000000000000000 ) ) ;
#19132 = CARTESIAN_POINT ( 'NONE',  ( -1.407845757905374695, -9.114917468222230923, 2.372643865078341019 ) ) ;
#19133 = CARTESIAN_POINT ( 'NONE',  ( 15.50000000000001776, -17.49999999999999645, 4.000000000000000000 ) ) ;
#19134 = CARTESIAN_POINT ( 'NONE',  ( -9.996558582316794173, -22.05068747287764452, 1.749999999999998446 ) ) ;
#19135 = AXIS2_PLACEMENT_3D ( 'NONE', #14498, #6770, #3213 ) ;
#19136 =( NAMED_UNIT ( * ) SI_UNIT ( $, .STERADIAN. ) SOLID_ANGLE_UNIT ( ) );
#19137 = CARTESIAN_POINT ( 'NONE',  ( 6.440941417683175629, -20.19639159124061933, 1.768074502826635586 ) ) ;
#19138 = DIRECTION ( 'NONE',  ( -1.000000000000000000, 0.000000000000000000, 0.000000000000000000 ) ) ;
#19139 = EDGE_CURVE ( 'NONE', #6961, #7639, #8804, .T. ) ;
#19140 = CARTESIAN_POINT ( 'NONE',  ( -5.972191417683179182, -23.72900456129165292, 2.724438792969417822 ) ) ;
#19141 = ORIENTED_EDGE ( 'NONE', *, *, #18871, .T. ) ;
#19142 = CARTESIAN_POINT ( 'NONE',  ( 7.934058582316792396, -23.20159541128345992, 4.773278322869455970 ) ) ;
#19143 = DIRECTION ( 'NONE',  ( 0.000000000000000000, 1.000000000000000000, -0.000000000000000000 ) ) ;
#19144 = CARTESIAN_POINT ( 'NONE',  ( -13.90439735423812273, 5.734566389025032684, 2.999999999999999556 ) ) ;
#19145 = CARTESIAN_POINT ( 'NONE',  ( 5.027808582316793284, -23.72900456129165647, 4.275561207030568411 ) ) ;
#19146 = LINE ( 'NONE', #14518, #302 ) ;
#19147 = VERTEX_POINT ( 'NONE', #16530 ) ;
#19148 = DIRECTION ( 'NONE',  ( 0.000000000000000000, 0.1264857625231113059, 0.9919684228235025047 ) ) ;
#19149 = ORIENTED_EDGE ( 'NONE', *, *, #7123, .T. ) ;
#19150 = VECTOR ( 'NONE', #658, 1000.000000000000000 ) ;
#19151 = ADVANCED_FACE ( 'NONE', ( #13593 ), #7134, .T. ) ;
#19152 = DIRECTION ( 'NONE',  ( 0.000000000000000000, 1.000000000000000000, -0.000000000000000000 ) ) ;
#19153 = EDGE_CURVE ( 'NONE', #7462, #6837, #13498, .T. ) ;
#19154 = EDGE_LOOP ( 'NONE', ( #2265, #18785, #12606, #3587 ) ) ;
#19155 = CARTESIAN_POINT ( 'NONE',  ( -6.527808582316794173, -23.72900456129165647, 4.275561207030568411 ) ) ;
#19156 = CARTESIAN_POINT ( 'NONE',  ( 12.64387510712649565, -19.29680709011273976, 5.506486987317513737 ) ) ;
#19157 = EDGE_CURVE ( 'NONE', #11568, #3392, #9208, .T. ) ;
#19158 = CARTESIAN_POINT ( 'NONE',  ( 4.000000000000000000, -12.50000000000000000, 3.464723819589916154 ) ) ;
#19159 = CARTESIAN_POINT ( 'NONE',  ( 1.859341899742023463, -9.902476528685241419, 1.632289782122827271 ) ) ;
#19160 = DIRECTION ( 'NONE',  ( 1.000000000000000000, 0.000000000000000000, -0.000000000000000000 ) ) ;
#19161 = CARTESIAN_POINT ( 'NONE',  ( -13.84074239313819277, 4.019990853478630832, 5.241358430878110930 ) ) ;
#19162 = CARTESIAN_POINT ( 'NONE',  ( 6.059058582316793284, -20.72672167713054137, 4.701595411283463477 ) ) ;
#19163 = CARTESIAN_POINT ( 'NONE',  ( -12.68302225826488616, -18.06987595762608478, 6.282912912489355683 ) ) ;
#19164 = VECTOR ( 'NONE', #2176, 1000.000000000000000 ) ;
#19165 = EDGE_CURVE ( 'NONE', #8626, #8041, #9663, .T. ) ;
#19166 = CARTESIAN_POINT ( 'NONE',  ( 17.30017143803810242, 9.000000000000001776, 0.000000000000000000 ) ) ;
#19167 = CARTESIAN_POINT ( 'NONE',  ( -9.996558582316795949, -22.05068747287764452, 0.9999999999999978906 ) ) ;
#19168 = CARTESIAN_POINT ( 'NONE',  ( 5.121558582316794173, -23.74999999999999645, 3.550687472877651629 ) ) ;
#19169 = CARTESIAN_POINT ( 'NONE',  ( 3.944195004867014909, -21.80034658733847053, 4.481176709221804444 ) ) ;
#19170 = CARTESIAN_POINT ( 'NONE',  ( -4.190941417683176518, -23.27327832286946219, 4.701595411283453707 ) ) ;
#19171 = VERTEX_POINT ( 'NONE', #15580 ) ;
#19172 = CARTESIAN_POINT ( 'NONE',  ( 13.84476264919594612, 4.223013784394161974, 5.079233071712400793 ) ) ;
#19173 = FACE_OUTER_BOUND ( 'NONE', #19096, .T. ) ;
#19174 = ORIENTED_EDGE ( 'NONE', *, *, #1281, .T. ) ;
#19175 = EDGE_LOOP ( 'NONE', ( #10805, #2851, #104, #9280 ) ) ;
#19176 = CARTESIAN_POINT ( 'NONE',  ( 11.99178095869207006, 4.999999999999999112, 1.000000000000000000 ) ) ;
#19177 = PRODUCT_DEFINITION ( 'UNKNOWN', '', #5035, #12560 ) ;
#19178 = DIRECTION ( 'NONE',  ( 1.000000000000000000, 0.000000000000000000, -0.000000000000000000 ) ) ;
#19179 = LINE ( 'NONE', #4832, #7260 ) ;
#19180 = CARTESIAN_POINT ( 'NONE',  ( -3.422464802389687311, -10.54865018547243061, 2.933470051312085936 ) ) ;
#19181 = PLANE ( 'NONE',  #8024 ) ;
#19182 = DIRECTION ( 'NONE',  ( 0.1351665943404306014, -0.9596796555888912339, 0.2464649070825229438 ) ) ;
#19183 = CARTESIAN_POINT ( 'NONE',  ( -13.10821839766814279, 4.152529082241303904, 5.997503362667785609 ) ) ;
#19184 = CARTESIAN_POINT ( 'NONE',  ( 13.27780858231679595, -20.27099543870833642, 2.724438792969431589 ) ) ;
#19185 = CARTESIAN_POINT ( 'NONE',  ( 5.381197846483058989, -14.00000000000000000, 1.000000000000000000 ) ) ;
#19186 = CARTESIAN_POINT ( 'NONE',  ( 13.11644927503132330, 3.818188389080370282, 6.753616037489316604 ) ) ;
#19187 = CARTESIAN_POINT ( 'NONE',  ( -1.863950040896528604, -9.995453039732266731, 2.406168007552154098 ) ) ;
#19188 = ORIENTED_EDGE ( 'NONE', *, *, #13469, .F. ) ;
#19189 = CARTESIAN_POINT ( 'NONE',  ( -13.87467358130843387, 4.983515856073828409, 5.065827972856573602 ) ) ;
#19190 = LINE ( 'NONE', #14353, #2361 ) ;
#19191 = ADVANCED_FACE ( 'NONE', ( #10574 ), #17510, .T. ) ;
#19192 = CARTESIAN_POINT ( 'NONE',  ( 7.472191417683177406, -24.47900456129165292, 2.413778621189595963 ) ) ;
#19193 = CARTESIAN_POINT ( 'NONE',  ( -4.940941417683177406, -21.25705176302044208, 2.828734674606458555 ) ) ;
#19194 = ORIENTED_EDGE ( 'NONE', *, *, #3855, .F. ) ;
#19195 = CARTESIAN_POINT ( 'NONE',  ( 12.62499963760179256, -21.00001830110826972, 4.442557003548452066 ) ) ;
#19196 = CARTESIAN_POINT ( 'NONE',  ( 13.12529397354238192, 5.014845663890295846, 4.666666666666619889 ) ) ;
#19197 = PLANE ( 'NONE',  #2659 ) ;
#19198 = ORIENTED_EDGE ( 'NONE', *, *, #13059, .F. ) ;
#19199 = ORIENTED_EDGE ( 'NONE', *, *, #4292, .T. ) ;
#19200 = DIRECTION ( 'NONE',  ( -1.000000000000000000, -1.734723475976787570E-15, 0.000000000000000000 ) ) ;
#19201 = LINE ( 'NONE', #7894, #9228 ) ;
#19202 = DIRECTION ( 'NONE',  ( 0.000000000000000000, -1.000000000000000000, 0.000000000000000000 ) ) ;
#19203 = CARTESIAN_POINT ( 'NONE',  ( -14.56494360078803396, 10.00000000000000000, 1.000000000000000000 ) ) ;
#19204 = DIRECTION ( 'NONE',  ( -0.000000000000000000, -0.000000000000000000, -1.000000000000000000 ) ) ;
#19205 = CARTESIAN_POINT ( 'NONE',  ( 2.081625295426255295, -10.37614485793134556, 1.753937271548854815 ) ) ;
#19206 = PLANE ( 'NONE',  #1850 ) ;
#19207 = CARTESIAN_POINT ( 'NONE',  ( 2.693754455098655409, -9.955255285363838524, 2.600628789231445470 ) ) ;
#19208 = DIRECTION ( 'NONE',  ( 0.1351665943404306014, -0.9596796555888912339, 0.2464649070825229438 ) ) ;
#19209 = LINE ( 'NONE', #20673, #628 ) ;
#19210 = DIRECTION ( 'NONE',  ( 0.000000000000000000, 0.000000000000000000, 1.000000000000000000 ) ) ;
#19211 = CARTESIAN_POINT ( 'NONE',  ( -0.1250000000000001110, 11.64110105645932691, 0.000000000000000000 ) ) ;
#19212 = PRODUCT ( 'spring housing', 'spring housing', '', ( #6886 ) ) ;
#19213 = CARTESIAN_POINT ( 'NONE',  ( 10.27780858231679595, -21.02099543870833998, 3.035098964749253003 ) ) ;
#19214 = CARTESIAN_POINT ( 'NONE',  ( -13.09073190589589331, 4.019461247742575516, 5.257453802652931607 ) ) ;
#19215 = CARTESIAN_POINT ( 'NONE',  ( -13.37155858231679417, -20.24999999999999289, 3.449312527122348371 ) ) ;
#19216 = EDGE_CURVE ( 'NONE', #10614, #7438, #16845, .T. ) ;
#19217 = CARTESIAN_POINT ( 'NONE',  ( -4.659691417683177406, -22.98484643305507191, 0.9790045612916508100 ) ) ;
#19218 = VERTEX_POINT ( 'NONE', #18417 ) ;
#19219 = CARTESIAN_POINT ( 'NONE',  ( 13.38569699238614952, -18.95980188449660986, 4.749177046715717054 ) ) ;
#19220 = CARTESIAN_POINT ( 'NONE',  ( -26.94203811574920593, 0.000000000000000000, 1.000000000000000000 ) ) ;
#19221 = ORIENTED_EDGE ( 'NONE', *, *, #1732, .F. ) ;
#19222 = ORIENTED_EDGE ( 'NONE', *, *, #16512, .T. ) ;
#19223 = CARTESIAN_POINT ( 'NONE',  ( 0.000000000000000000, 4.999999999999999112, 0.000000000000000000 ) ) ;
#19224 = VERTEX_POINT ( 'NONE', #7324 ) ;
#19225 = DIRECTION ( 'NONE',  ( 0.000000000000000000, 1.000000000000000000, 0.000000000000000000 ) ) ;
#19226 = EDGE_CURVE ( 'NONE', #13134, #3417, #19672, .T. ) ;
#19227 = EDGE_CURVE ( 'NONE', #2846, #7153, #13487, .T. ) ;
#19228 = AXIS2_PLACEMENT_3D ( 'NONE', #13013, #3195, #10939 ) ;
#19229 = EDGE_LOOP ( 'NONE', ( #9605, #9489, #17103, #1824 ) ) ;
#19230 = CARTESIAN_POINT ( 'NONE',  ( 9.253441417683177406, -21.94931252712233061, 1.749999999999998446 ) ) ;
#19231 = VECTOR ( 'NONE', #3570, 1000.000000000000000 ) ;
#19232 = CARTESIAN_POINT ( 'NONE',  ( -2.203959450683124377, -9.262433282444222371, 2.410528873095051594 ) ) ;
#19233 = FACE_OUTER_BOUND ( 'NONE', #4748, .T. ) ;
#19234 = CARTESIAN_POINT ( 'NONE',  ( -2.499999999999998668, -19.50000000000000000, 4.000000000000000000 ) ) ;
#19235 = VECTOR ( 'NONE', #6106, 1000.000000000000000 ) ;
#19236 = DIRECTION ( 'NONE',  ( -0.000000000000000000, -0.000000000000000000, -1.000000000000000000 ) ) ;
#19237 = CARTESIAN_POINT ( 'NONE',  ( 10.47219141768317563, -23.72900456129165292, 2.724438792969417822 ) ) ;
#19238 = DIRECTION ( 'NONE',  ( -0.000000000000000000, -0.000000000000000000, -1.000000000000000000 ) ) ;
#19239 = CARTESIAN_POINT ( 'NONE',  ( -11.87844141768317741, -22.99999999999999645, 3.449312527122335048 ) ) ;
#19240 = EDGE_CURVE ( 'NONE', #3754, #346, #11985, .T. ) ;
#19241 = ORIENTED_EDGE ( 'NONE', *, *, #11128, .T. ) ;
#19242 = CARTESIAN_POINT ( 'NONE',  ( 11.59030858231679595, -21.01515356694490322, 0.9790045612916562501 ) ) ;
#19243 = CARTESIAN_POINT ( 'NONE',  ( -27.50000000000000711, 4.999999999999999112, 1.000000000000000000 ) ) ;
#19244 = CARTESIAN_POINT ( 'NONE',  ( -12.62499999999998401, -20.99999999999999645, 3.146526952850934755 ) ) ;
#19245 = ORIENTED_EDGE ( 'NONE', *, *, #18846, .F. ) ;
#19246 = CARTESIAN_POINT ( 'NONE',  ( 6.059058582316793284, -20.72672167713054137, 4.701595411283463477 ) ) ;
#19247 = LINE ( 'NONE', #1969, #15000 ) ;
#19248 = ORIENTED_EDGE ( 'NONE', *, *, #5501, .F. ) ;
#19249 = CARTESIAN_POINT ( 'NONE',  ( 32.65117217603048516, 6.460468870412194420, 1.000000000000000000 ) ) ;
#19250 = VERTEX_POINT ( 'NONE', #2195 ) ;
#19251 = CARTESIAN_POINT ( 'NONE',  ( 13.42791111847407848, 9.000000000000001776, 1.000000000000000000 ) ) ;
#19252 = EDGE_LOOP ( 'NONE', ( #11995, #3722, #12362, #13032, #655, #6307, #14294, #10863, #6046, #1249, #11182, #3973, #12213, #17849, #8710, #16641, #14697, #11156, #18503, #9811, #6372, #15284, #15059, #8933, #20569, #10956, #8875, #1723, #17087, #14181, #5253, #17631, #1365, #17283, #13029, #5572, #19622, #20323, #19627, #4109, #2053, #19890, #1598, #13225, #19459, #12918, #7937, #12610, #17995, #14593, #12529, #16453, #6459, #13365, #6074, #10694, #18729, #4208, #5473, #12516, #3691, #9482, #13898, #4646, #4396, #2348, #1342, #20302, #13512, #10415, #1810, #10779, #5800, #16665, #15778, #9501, #3013, #245, #18813, #5087, #9896, #15852, #2634, #17824, #9294, #12849, #13852, #16760, #6111, #1500, #6762, #14257, #9796, #14678, #9384, #3306, #17342, #5423, #17069, #3131, #18340, #11915, #14274, #11692, #7100, #19618, #5134, #2325, #12026, #20687, #4241, #3303, #12286, #991, #11796, #13247, #4723, #18782, #15733, #629, #11092, #9225, #1295, #1156 ) ) ;
#19253 = EDGE_CURVE ( 'NONE', #19324, #4668, #4181, .T. ) ;
#19254 = CARTESIAN_POINT ( 'NONE',  ( -4.746558582316793284, -21.94931252712234482, 5.250000000000000888 ) ) ;
#19255 = LINE ( 'NONE', #6588, #5250 ) ;
#19256 = FACE_OUTER_BOUND ( 'NONE', #18826, .T. ) ;
#19257 = CARTESIAN_POINT ( 'NONE',  ( 2.049450250860079592, -10.15122911285664564, 1.696174415070213382 ) ) ;
#19258 = CARTESIAN_POINT ( 'NONE',  ( 12.65650603190776025, -18.65894538865861563, 5.520212342915047365 ) ) ;
#19259 = DIRECTION ( 'NONE',  ( 0.000000000000000000, -0.000000000000000000, 1.000000000000000000 ) ) ;
#19260 = CARTESIAN_POINT ( 'NONE',  ( -13.39888564296547635, -18.29377503024027263, 4.763499963382565205 ) ) ;
#19261 = CARTESIAN_POINT ( 'NONE',  ( 8.215308582316792396, -23.77099543870833998, 2.825813738724734847 ) ) ;
#19262 = CARTESIAN_POINT ( 'NONE',  ( -12.65457057572495181, -19.50668592589112293, 6.238308001337955488 ) ) ;
#19263 = ADVANCED_FACE ( 'NONE', ( #8995 ), #5758, .F. ) ;
#19264 = EDGE_CURVE ( 'NONE', #13151, #15413, #6904, .T. ) ;
#19265 = DIRECTION ( 'NONE',  ( 1.000000000000000000, 0.000000000000000000, 0.000000000000000000 ) ) ;
#19266 = CARTESIAN_POINT ( 'NONE',  ( -9.340308582316795949, -22.98484643305508612, 6.020995438708344416 ) ) ;
#19267 = CARTESIAN_POINT ( 'NONE',  ( 5.965308582316793284, -20.22900456129164937, 4.174186261275266929 ) ) ;
#19268 = CARTESIAN_POINT ( 'NONE',  ( 6.909691417683176518, -21.63647391050456648, 4.520995438708348857 ) ) ;
#19269 = CARTESIAN_POINT ( 'NONE',  ( -6.159691417683176518, -22.67418626127524917, 1.729004561291651587 ) ) ;
#19270 = EDGE_LOOP ( 'NONE', ( #10384, #8837, #17149, #3644 ) ) ;
#19271 = EDGE_LOOP ( 'NONE', ( #10545, #3039, #14228, #11867 ) ) ;
#19272 = CARTESIAN_POINT ( 'NONE',  ( 13.84256985046264710, 4.112277448363203192, 5.213861325540929847 ) ) ;
#19273 = DIRECTION ( 'NONE',  ( 1.000000000000000000, 0.000000000000000000, -0.000000000000000000 ) ) ;
#19274 = DIRECTION ( 'NONE',  ( -1.000000000000000000, 0.000000000000000000, 0.000000000000000000 ) ) ;
#19275 = VERTEX_POINT ( 'NONE', #10150 ) ;
#19276 = EDGE_LOOP ( 'NONE', ( #12340, #17293, #19485, #1585 ) ) ;
#19277 = LINE ( 'NONE', #6194, #16787 ) ;
#19278 = VECTOR ( 'NONE', #5371, 1000.000000000000000 ) ;
#19279 = DIRECTION ( 'NONE',  ( 0.000000000000000000, 0.000000000000000000, -1.000000000000000000 ) ) ;
#19280 = ADVANCED_FACE ( 'NONE', ( #5337 ), #13272, .F. ) ;
#19281 = DIRECTION ( 'NONE',  ( -0.7071067811865474617, -0.000000000000000000, 0.7071067811865474617 ) ) ;
#19282 = CARTESIAN_POINT ( 'NONE',  ( -1.884282074604925583, -8.375506800461993251, 2.375363417140690547 ) ) ;
#19283 = DIRECTION ( 'NONE',  ( 0.000000000000000000, -1.000000000000000000, 0.000000000000000000 ) ) ;
#19284 = DIRECTION ( 'NONE',  ( 1.156482317317871971E-16, -1.000000000000000000, 0.000000000000000000 ) ) ;
#19285 = CARTESIAN_POINT ( 'NONE',  ( -13.12119116326504908, 4.807653744879115010, 5.626470997801169105 ) ) ;
#19286 = CARTESIAN_POINT ( 'NONE',  ( 12.34030858231679240, -22.67418626127525982, 5.270995438708342640 ) ) ;
#19287 = DIRECTION ( 'NONE',  ( -0.000000000000000000, -0.000000000000000000, -1.000000000000000000 ) ) ;
#19288 = CARTESIAN_POINT ( 'NONE',  ( 12.62500000000001954, -20.24999999999450040, 3.833333333368183382 ) ) ;
#19289 = CARTESIAN_POINT ( 'NONE',  ( -2.557403344953185442, -14.91030650174552896, 3.668400560659690779 ) ) ;
#19290 = ORIENTED_EDGE ( 'NONE', *, *, #6440, .T. ) ;
#19291 = AXIS2_PLACEMENT_3D ( 'NONE', #13416, #14882, #560 ) ;
#19292 = CARTESIAN_POINT ( 'NONE',  ( -13.85343352903393388, 3.910893216212274925, 5.991044282956552891 ) ) ;
#19293 = CARTESIAN_POINT ( 'NONE',  ( -24.79469207716615031, 4.999999999999999112, 0.000000000000000000 ) ) ;
#19294 = CARTESIAN_POINT ( 'NONE',  ( 4.940941417683177406, -20.19639159124061933, 1.768074502826635586 ) ) ;
#19295 = CARTESIAN_POINT ( 'NONE',  ( -9.996558582316795949, -22.05068747287764452, 2.499999999999999112 ) ) ;
#19296 = EDGE_LOOP ( 'NONE', ( #20535, #8438, #13126, #19577 ) ) ;
#19297 = CARTESIAN_POINT ( 'NONE',  ( 12.62927505847832776, -20.78410954684871825, 5.373974324164845662 ) ) ;
#19298 = CARTESIAN_POINT ( 'NONE',  ( 13.12424783836753228, 4.962015837561366993, 5.328858059679200565 ) ) ;
#19299 = LINE ( 'NONE', #8204, #2327 ) ;
#19300 = ORIENTED_EDGE ( 'NONE', *, *, #5565, .F. ) ;
#19301 = ORIENTED_EDGE ( 'NONE', *, *, #10013, .T. ) ;
#19302 = CARTESIAN_POINT ( 'NONE',  ( 27.00000000000000000, 0.000000000000000000, 1.000000000000000000 ) ) ;
#19303 = EDGE_CURVE ( 'NONE', #7476, #19147, #4079, .T. ) ;
#19304 = DIRECTION ( 'NONE',  ( 0.000000000000000000, -0.000000000000000000, 1.000000000000000000 ) ) ;
#19305 = ORIENTED_EDGE ( 'NONE', *, *, #7980, .T. ) ;
#19306 = CARTESIAN_POINT ( 'NONE',  ( -3.997260319564023501, 0.000000000000000000, 1.000000000000000000 ) ) ;
#19307 = CARTESIAN_POINT ( 'NONE',  ( 1.896776615114361908, -10.21987218505477024, 2.463803327293850209 ) ) ;
#19308 = DIRECTION ( 'NONE',  ( -0.000000000000000000, 0.000000000000000000, -1.000000000000000000 ) ) ;
#19309 = VECTOR ( 'NONE', #19872, 1000.000000000000000 ) ;
#19310 = DIRECTION ( 'NONE',  ( 0.1351665943404306014, -0.9596796555888911229, 0.2464649070825229160 ) ) ;
#19311 = LINE ( 'NONE', #6544, #9697 ) ;
#19312 = DIRECTION ( 'NONE',  ( 0.000000000000000000, 0.000000000000000000, 1.000000000000000000 ) ) ;
#19313 = DIRECTION ( 'NONE',  ( -1.000000000000000000, -0.000000000000000000, -0.000000000000000000 ) ) ;
#19314 = PLANE ( 'NONE',  #14018 ) ;
#19315 = CARTESIAN_POINT ( 'NONE',  ( -13.09455366754861139, 4.212460211200554916, 5.160171780694988719 ) ) ;
#19316 = CARTESIAN_POINT ( 'NONE',  ( -12.80905858231679417, -23.27327832286945153, 2.298404588716537411 ) ) ;
#19317 = CARTESIAN_POINT ( 'NONE',  ( -8.315941417683177406, -20.79840458871654363, 4.773278322869464851 ) ) ;
#19318 = ORIENTED_EDGE ( 'NONE', *, *, #3496, .T. ) ;
#19319 = CARTESIAN_POINT ( 'NONE',  ( 13.37847682517167947, -19.32442032882675775, 4.733786629989340078 ) ) ;
#19320 = LINE ( 'NONE', #4977, #11704 ) ;
#19321 = ORIENTED_EDGE ( 'NONE', *, *, #18837, .F. ) ;
#19322 = VERTEX_POINT ( 'NONE', #8686 ) ;
#19323 = DIRECTION ( 'NONE',  ( 1.000000000000000000, 0.000000000000000000, 0.000000000000000000 ) ) ;
#19324 = VERTEX_POINT ( 'NONE', #15057 ) ;
#19325 = DIRECTION ( 'NONE',  ( -2.312964634635756072E-15, 1.000000000000000000, 0.000000000000000000 ) ) ;
#19326 = VECTOR ( 'NONE', #4158, 1000.000000000000000 ) ;
#19327 = ORIENTED_EDGE ( 'NONE', *, *, #2619, .F. ) ;
#19328 = CARTESIAN_POINT ( 'NONE',  ( 11.03469141768317918, -20.22900456129164581, 2.825813738724748170 ) ) ;
#19329 = DIRECTION ( 'NONE',  ( -1.000000000000000000, 0.000000000000000000, 0.000000000000000000 ) ) ;
#19330 = EDGE_CURVE ( 'NONE', #11328, #15500, #8578, .T. ) ;
#19331 = LINE ( 'NONE', #4989, #18670 ) ;
#19332 = CARTESIAN_POINT ( 'NONE',  ( -13.17791111847408025, 4.999999999999999112, 1.000000000000000000 ) ) ;
#19333 = CARTESIAN_POINT ( 'NONE',  ( -9.715308582316794173, -23.77099543870833998, 2.825813738724734847 ) ) ;
#19334 = VECTOR ( 'NONE', #3990, 1000.000000000000000 ) ;
#19335 = CARTESIAN_POINT ( 'NONE',  ( 0.000000000000000000, 9.000000000000001776, 0.000000000000000000 ) ) ;
#19336 = EDGE_CURVE ( 'NONE', #3190, #15518, #7016, .T. ) ;
#19337 = ADVANCED_FACE ( 'NONE', ( #19786 ), #8894, .T. ) ;
#19338 = CARTESIAN_POINT ( 'NONE',  ( 9.065941417683177406, -23.20159541128344927, 2.226721677130534705 ) ) ;
#19339 = DIRECTION ( 'NONE',  ( 0.000000000000000000, 1.000000000000000000, -0.000000000000000000 ) ) ;
#19340 = CARTESIAN_POINT ( 'NONE',  ( -10.75344141768317741, -21.94931252712233061, 2.499999999999999112 ) ) ;
#19341 = VERTEX_POINT ( 'NONE', #15260 ) ;
#19342 = CARTESIAN_POINT ( 'NONE',  ( 10.09030858231679595, -21.01515356694490322, 0.9790045612916562501 ) ) ;
#19343 = CARTESIAN_POINT ( 'NONE',  ( 13.11017182064853159, 4.251176942750957366, 5.979809059808775196 ) ) ;
#19344 = CARTESIAN_POINT ( 'NONE',  ( -13.10745701327265778, 3.364079170269163921, 6.743850412489304169 ) ) ;
#19345 = ORIENTED_EDGE ( 'NONE', *, *, #20443, .F. ) ;
#19346 = DIRECTION ( 'NONE',  ( 0.000000000000000000, 0.000000000000000000, -1.000000000000000000 ) ) ;
#19347 = CARTESIAN_POINT ( 'NONE',  ( -17.55017143803810242, 0.000000000000000000, 1.000000000000000000 ) ) ;
#19348 = ORIENTED_EDGE ( 'NONE', *, *, #7387, .T. ) ;
#19349 = AXIS2_PLACEMENT_3D ( 'NONE', #4214, #18346, #4010 ) ;
#19350 = ORIENTED_EDGE ( 'NONE', *, *, #6908, .F. ) ;
#19351 = VECTOR ( 'NONE', #16872, 1000.000000000000000 ) ;
#19352 = DIRECTION ( 'NONE',  ( 6.938893903907228378E-16, -1.000000000000000000, 0.000000000000000000 ) ) ;
#19353 = AXIS2_PLACEMENT_3D ( 'NONE', #4165, #20282, #12313 ) ;
#19354 = VERTEX_POINT ( 'NONE', #3869 ) ;
#19355 = CARTESIAN_POINT ( 'NONE',  ( -12.15280858231679950, -20.91377862118960351, 5.979004561291660913 ) ) ;
#19356 = CARTESIAN_POINT ( 'NONE',  ( 12.62499999999998224, -20.25000000000006395, 4.416666666666681174 ) ) ;
#19357 = EDGE_CURVE ( 'NONE', #17356, #13797, #18207, .T. ) ;
#19358 = LINE ( 'NONE', #14313, #14134 ) ;
#19359 = CARTESIAN_POINT ( 'NONE',  ( 2.081625295426255295, -10.37614485793134556, 1.753937271548854815 ) ) ;
#19360 = CARTESIAN_POINT ( 'NONE',  ( 13.06655316810189227, 2.048434989138931961, 5.965524842914772030 ) ) ;
#19361 = DIRECTION ( 'NONE',  ( -1.000000000000000000, 0.000000000000000000, 0.000000000000000000 ) ) ;
#19362 = CARTESIAN_POINT ( 'NONE',  ( -13.57153706873194032, -9.574878029060977624, 4.950999963380944280 ) ) ;
#19363 = AXIS2_PLACEMENT_3D ( 'NONE', #17926, #19515, #6749 ) ;
#19364 = CARTESIAN_POINT ( 'NONE',  ( 10.37155858231679595, -19.49999999999998934, 3.449312527122348371 ) ) ;
#19365 = CARTESIAN_POINT ( 'NONE',  ( -13.11644927503132330, 3.818188389080370282, 6.753616037489316604 ) ) ;
#19366 = AXIS2_PLACEMENT_3D ( 'NONE', #8770, #16593, #816 ) ;
#19367 = DIRECTION ( 'NONE',  ( 1.000000000000000000, 1.192622389734054877E-16, -0.000000000000000000 ) ) ;
#19368 = DIRECTION ( 'NONE',  ( 2.312964634635731617E-15, -1.000000000000000000, 0.000000000000000000 ) ) ;
#19369 = VECTOR ( 'NONE', #20586, 1000.000000000000000 ) ;
#19370 = EDGE_CURVE ( 'NONE', #12022, #19576, #938, .T. ) ;
#19371 = CARTESIAN_POINT ( 'NONE',  ( 10.09030858231679595, -21.63647391050454871, 2.479004561291657804 ) ) ;
#19372 = CARTESIAN_POINT ( 'NONE',  ( -6.253441417683176518, -21.94931252712233061, 1.749999999999998446 ) ) ;
#19373 = ORIENTED_EDGE ( 'NONE', *, *, #7251, .T. ) ;
#19374 = ORIENTED_EDGE ( 'NONE', *, *, #10896, .F. ) ;
#19375 = CARTESIAN_POINT ( 'NONE',  ( 13.37500000000002132, -20.25000000000274269, 4.083333333315724012 ) ) ;
#19376 = LINE ( 'NONE', #16125, #4476 ) ;
#19377 = EDGE_LOOP ( 'NONE', ( #3972, #10358, #244, #2474 ) ) ;
#19378 = EDGE_LOOP ( 'NONE', ( #17658, #4340, #16678, #14807 ) ) ;
#19379 = DIRECTION ( 'NONE',  ( 0.000000000000000000, 1.000000000000000000, -0.000000000000000000 ) ) ;
#19380 = LINE ( 'NONE', #9636, #11690 ) ;
#19381 = CARTESIAN_POINT ( 'NONE',  ( -13.12512971825177033, 5.006550771716304915, 5.133277049491872468 ) ) ;
#19382 = EDGE_CURVE ( 'NONE', #12385, #13259, #3970, .T. ) ;
#19383 = AXIS2_PLACEMENT_3D ( 'NONE', #6404, #12770, #4420 ) ;
#19384 = ADVANCED_FACE ( 'NONE', ( #15163 ), #13686, .T. ) ;
#19385 = LINE ( 'NONE', #20570, #6858 ) ;
#19386 = CARTESIAN_POINT ( 'NONE',  ( -2.708677329869237482, -9.785633270066144362, 1.794897081886200230 ) ) ;
#19387 = VECTOR ( 'NONE', #6799, 1000.000000000000000 ) ;
#19388 = DIRECTION ( 'NONE',  ( -1.000000000000000000, 0.000000000000000000, 0.000000000000000000 ) ) ;
#19389 = CARTESIAN_POINT ( 'NONE',  ( -13.12424783836753228, 4.962015837561366993, 5.328858059679200565 ) ) ;
#19390 = SURFACE_STYLE_FILL_AREA ( #5461 ) ;
#19391 = DIRECTION ( 'NONE',  ( 1.000000000000000000, 0.000000000000000000, -0.000000000000000000 ) ) ;
#19392 = CARTESIAN_POINT ( 'NONE',  ( 12.64387510712649565, -19.29680709011273976, 5.506486987317513737 ) ) ;
#19393 = DIRECTION ( 'NONE',  ( 0.000000000000000000, 1.000000000000000000, -0.000000000000000000 ) ) ;
#19394 = VECTOR ( 'NONE', #1805, 1000.000000000000000 ) ;
#19395 = EDGE_LOOP ( 'NONE', ( #355, #13585, #20486, #14179 ) ) ;
#19396 = CARTESIAN_POINT ( 'NONE',  ( -13.39542766346049518, -19.21840299524461315, 5.493648449623241170 ) ) ;
#19397 = LINE ( 'NONE', #4634, #3369 ) ;
#19398 = CARTESIAN_POINT ( 'NONE',  ( 7.284691417683176518, -24.52099543870834708, 4.484846433055073689 ) ) ;
#19399 = CARTESIAN_POINT ( 'NONE',  ( -9.809058582316795949, -22.74294823697954016, 2.828734674606448785 ) ) ;
#19400 = COLOUR_RGB ( '', 0.66274510, 0.83137255, 0.94901961) ;
#19401 = ORIENTED_EDGE ( 'NONE', *, *, #1493, .T. ) ;
#19402 = CARTESIAN_POINT ( 'NONE',  ( 13.88684657106908205, 4.848251838987907014, 6.535242036940271504 ) ) ;
#19403 = CARTESIAN_POINT ( 'NONE',  ( 12.64387510712649565, -19.29680709011273976, 5.506486987317513737 ) ) ;
#19404 = FACE_OUTER_BOUND ( 'NONE', #5523, .T. ) ;
#19405 = ORIENTED_EDGE ( 'NONE', *, *, #927, .F. ) ;
#19406 = VECTOR ( 'NONE', #1733, 1000.000000000000000 ) ;
#19407 = VERTEX_POINT ( 'NONE', #20095 ) ;
#19408 = DIRECTION ( 'NONE',  ( -0.000000000000000000, -0.000000000000000000, -1.000000000000000000 ) ) ;
#19409 = CARTESIAN_POINT ( 'NONE',  ( 4.315753587183824180, -21.65797192216093947, 4.831781436261117335 ) ) ;
#19410 = EDGE_CURVE ( 'NONE', #12443, #11466, #4495, .T. ) ;
#19411 = DIRECTION ( 'NONE',  ( -0.000000000000000000, -1.000000000000000000, -0.000000000000000000 ) ) ;
#19412 = LINE ( 'NONE', #19306, #18684 ) ;
#19413 = CARTESIAN_POINT ( 'NONE',  ( 1.126276606324276619, -9.114917468222230923, 1.622643865078341463 ) ) ;
#19414 = CARTESIAN_POINT ( 'NONE',  ( 4.999999999999998224, -2.500000000000047518, 9.999999999999998224 ) ) ;
#19415 = LINE ( 'NONE', #4860, #12764 ) ;
#19416 = VECTOR ( 'NONE', #993, 1000.000000000000000 ) ;
#19417 = AXIS2_PLACEMENT_3D ( 'NONE', #14773, #2137, #2233 ) ;
#19418 = DIRECTION ( 'NONE',  ( -0.000000000000000000, -0.000000000000000000, -1.000000000000000000 ) ) ;
#19419 = CARTESIAN_POINT ( 'NONE',  ( -4.315753587183824180, -21.65797192216093947, 4.831781436261117335 ) ) ;
#19420 = CARTESIAN_POINT ( 'NONE',  ( -11.75209451496117197, 11.64110105645932691, 0.000000000000000000 ) ) ;
#19421 = AXIS2_PLACEMENT_3D ( 'NONE', #1395, #17593, #12568 ) ;
#19422 = CARTESIAN_POINT ( 'NONE',  ( -3.162271481458107658, -13.95306990448253437, 3.615178062515473911 ) ) ;
#19423 = VERTEX_POINT ( 'NONE', #14201 ) ;
#19424 = CARTESIAN_POINT ( 'NONE',  ( -13.07840392524817474, 3.396898225032857432, 5.244490940007585422 ) ) ;
#19425 = CARTESIAN_POINT ( 'NONE',  ( -6.246558582316795949, -21.94931252712234127, 4.499999999999999112 ) ) ;
#19426 = EDGE_CURVE ( 'NONE', #911, #16884, #10667, .T. ) ;
#19427 = CARTESIAN_POINT ( 'NONE',  ( -9.440941417683177406, -20.72672167713052715, 2.298404588716546293 ) ) ;
#19428 = ORIENTED_EDGE ( 'NONE', *, *, #17435, .F. ) ;
#19429 = CARTESIAN_POINT ( 'NONE',  ( 13.38449802415168932, -19.02034978033825396, 4.747874963382372471 ) ) ;
#19430 = DIRECTION ( 'NONE',  ( -0.000000000000000000, -0.000000000000000000, -1.000000000000000000 ) ) ;
#19431 = ORIENTED_EDGE ( 'NONE', *, *, #16803, .F. ) ;
#19432 = ORIENTED_EDGE ( 'NONE', *, *, #16053, .T. ) ;
#19433 = LINE ( 'NONE', #9895, #10421 ) ;
#19434 = ORIENTED_EDGE ( 'NONE', *, *, #1207, .F. ) ;
#19435 = FACE_OUTER_BOUND ( 'NONE', #16732, .T. ) ;
#19436 = VECTOR ( 'NONE', #15895, 1000.000000000000000 ) ;
#19437 = VECTOR ( 'NONE', #8909, 1000.000000000000000 ) ;
#19438 = ORIENTED_EDGE ( 'NONE', *, *, #19227, .T. ) ;
#19439 = CARTESIAN_POINT ( 'NONE',  ( -11.75209451496117197, 0.000000000000000000, 1.000000000000000000 ) ) ;
#19440 = CARTESIAN_POINT ( 'NONE',  ( 0.000000000000000000, 4.999999999999999112, 1.000000000000000000 ) ) ;
#19441 = CARTESIAN_POINT ( 'NONE',  ( -1.513434189748285918, -9.864917468222230923, 2.372643865078341019 ) ) ;
#19442 = CARTESIAN_POINT ( 'NONE',  ( 0.000000000000000000, 9.000000000000001776, 1.000000000000000000 ) ) ;
#19443 = CARTESIAN_POINT ( 'NONE',  ( -9.621558582316794173, -23.74999999999999645, 3.550687472877651629 ) ) ;
#19444 = CARTESIAN_POINT ( 'NONE',  ( 6.440941417683176518, -20.72672167713052715, 2.298404588716546293 ) ) ;
#19445 = LINE ( 'NONE', #17958, #8874 ) ;
#19446 = CARTESIAN_POINT ( 'NONE',  ( -11.97219141768317918, -22.97900456129165292, 3.035098964749240125 ) ) ;
#19447 = VECTOR ( 'NONE', #93, 1000.000000000000000 ) ;
#19448 = ORIENTED_EDGE ( 'NONE', *, *, #11038, .T. ) ;
#19449 = CARTESIAN_POINT ( 'NONE',  ( 12.52780858231679773, -24.47900456129166358, 4.586221378810390270 ) ) ;
#19450 = CARTESIAN_POINT ( 'NONE',  ( 12.62503117662529739, -20.24842558042254836, 4.565011198945062354 ) ) ;
#19451 = CARTESIAN_POINT ( 'NONE',  ( -12.62524871736568954, -20.23743977303344010, 4.661898514667671023 ) ) ;
#19452 = ORIENTED_EDGE ( 'NONE', *, *, #9276, .T. ) ;
#19453 = ADVANCED_FACE ( 'NONE', ( #1154 ), #15571, .T. ) ;
#19454 = DIRECTION ( 'NONE',  ( 0.000000000000000000, 0.000000000000000000, -1.000000000000000000 ) ) ;
#19455 = LINE ( 'NONE', #11383, #3316 ) ;
#19456 = VECTOR ( 'NONE', #2336, 1000.000000000000000 ) ;
#19457 = VERTEX_POINT ( 'NONE', #3032 ) ;
#19458 =( LENGTH_UNIT ( ) NAMED_UNIT ( * ) SI_UNIT ( .MILLI., .METRE. ) );
#19459 = ORIENTED_EDGE ( 'NONE', *, *, #8511, .F. ) ;
#19460 = CARTESIAN_POINT ( 'NONE',  ( 13.32807253909975920, -20.06651685969616494, 3.455426783468704244 ) ) ;
#19461 = VERTEX_POINT ( 'NONE', #10880 ) ;
#19462 = CARTESIAN_POINT ( 'NONE',  ( -8.215308582316792396, -23.77099543870833998, 2.825813738724734847 ) ) ;
#19463 = VECTOR ( 'NONE', #17409, 1000.000000000000000 ) ;
#19464 = CARTESIAN_POINT ( 'NONE',  ( 12.68288333306630378, -17.32689168014509207, 5.548858176248425700 ) ) ;
#19465 = DIRECTION ( 'NONE',  ( 1.000000000000000000, 0.000000000000000000, 0.000000000000000000 ) ) ;
#19466 = COLOUR_RGB ( '', 0.31764706, 0.68627451, 0.89019608) ;
#19467 = CARTESIAN_POINT ( 'NONE',  ( 12.64511805349267526, -19.23403829861753422, 5.507852591554869726 ) ) ;
#19468 = DIRECTION ( 'NONE',  ( 0.000000000000000000, 0.000000000000000000, 1.000000000000000000 ) ) ;
#19469 = CARTESIAN_POINT ( 'NONE',  ( -13.37500000000002132, -20.25000000000274269, 4.083333333315724012 ) ) ;
#19470 = CARTESIAN_POINT ( 'NONE',  ( 11.77780858231679595, -19.52099543870833642, 2.413778621189609286 ) ) ;
#19471 = AXIS2_PLACEMENT_3D ( 'NONE', #1792, #15523, #13848 ) ;
#19472 = CARTESIAN_POINT ( 'NONE',  ( -13.02352923685845631, -0.8742735386340954040, 6.652704579156702991 ) ) ;
#19473 = CARTESIAN_POINT ( 'NONE',  ( -9.909691417683175629, -21.01515356694492098, 6.020995438708349745 ) ) ;
#19474 = DIRECTION ( 'NONE',  ( 0.000000000000000000, 1.000000000000000000, 0.000000000000000000 ) ) ;
#19475 = CARTESIAN_POINT ( 'NONE',  ( 15.00000000000001599, -18.49999999999999645, 4.000000000000000000 ) ) ;
#19476 = VECTOR ( 'NONE', #4110, 1000.000000000000000 ) ;
#19477 = ADVANCED_FACE ( 'NONE', ( #1361 ), #6167, .T. ) ;
#19478 = CARTESIAN_POINT ( 'NONE',  ( 12.24655858231679595, -21.94931252712234127, 4.499999999999999112 ) ) ;
#19479 = CARTESIAN_POINT ( 'NONE',  ( -7.378441417683176518, -23.74999999999999645, 3.449312527122335492 ) ) ;
#19480 = VERTEX_POINT ( 'NONE', #7531 ) ;
#19481 = EDGE_LOOP ( 'NONE', ( #7817, #8962, #17119, #6585 ) ) ;
#19482 = CARTESIAN_POINT ( 'NONE',  ( 13.84439157666246878, 4.204274621457510186, 5.123803251657143676 ) ) ;
#19483 = DIRECTION ( 'NONE',  ( -0.000000000000000000, -0.000000000000000000, -1.000000000000000000 ) ) ;
#19484 = DIRECTION ( 'NONE',  ( 0.4999999999999949485, -0.8660254037844415942, 0.000000000000000000 ) ) ;
#19485 = ORIENTED_EDGE ( 'NONE', *, *, #12681, .F. ) ;
#19486 = FACE_OUTER_BOUND ( 'NONE', #8688, .T. ) ;
#19487 = EDGE_CURVE ( 'NONE', #9004, #3619, #15781, .T. ) ;
#19488 = EDGE_CURVE ( 'NONE', #17662, #14732, #2980, .T. ) ;
#19489 = FACE_OUTER_BOUND ( 'NONE', #168, .T. ) ;
#19490 = CARTESIAN_POINT ( 'NONE',  ( 13.37499999999998224, -20.24999999999991829, 4.333333333333343695 ) ) ;
#19491 = CARTESIAN_POINT ( 'NONE',  ( 0.000000000000000000, 4.999999999999999112, 1.000000000000000000 ) ) ;
#19492 = EDGE_CURVE ( 'NONE', #10573, #20689, #6261, .T. ) ;
#19493 = VECTOR ( 'NONE', #2411, 1000.000000000000000 ) ;
#19494 = CARTESIAN_POINT ( 'NONE',  ( 1.548630333695928396, -9.114917468222230923, 1.622643865078341463 ) ) ;
#19495 = CARTESIAN_POINT ( 'NONE',  ( -12.62500016093973620, -20.24999187254239175, 4.532396751752561848 ) ) ;
#19496 = CARTESIAN_POINT ( 'NONE',  ( 4.717959273841178636, -21.72818306014730183, 5.243595146365860771 ) ) ;
#19497 = CARTESIAN_POINT ( 'NONE',  ( -1.437849085826860884, 0.000000000000000000, 1.000000000000000000 ) ) ;
#19498 = CARTESIAN_POINT ( 'NONE',  ( 13.12119116326504908, 4.807653744879115010, 5.626470997801169105 ) ) ;
#19499 = CARTESIAN_POINT ( 'NONE',  ( -2.109407804498405703, -9.207748739546751438, 2.396484790045401603 ) ) ;
#19500 = CARTESIAN_POINT ( 'NONE',  ( -13.84983662433050178, 3.729249528687784920, 5.987138032956566214 ) ) ;
#19501 = LINE ( 'NONE', #5154, #368 ) ;
#19502 = EDGE_CURVE ( 'NONE', #9491, #12176, #12634, .T. ) ;
#19503 = CARTESIAN_POINT ( 'NONE',  ( 8.315941417683177406, -20.79840458871654363, 4.773278322869464851 ) ) ;
#19504 = AXIS2_PLACEMENT_3D ( 'NONE', #2087, #8782, #5324 ) ;
#19505 = CARTESIAN_POINT ( 'NONE',  ( -8.684058582316795949, -21.32873467460644079, 2.757051763020455404 ) ) ;
#19506 = ORIENTED_EDGE ( 'NONE', *, *, #18955, .T. ) ;
#19507 = CARTESIAN_POINT ( 'NONE',  ( 12.62499999999998401, -20.99999999999998934, 2.439580858552613751 ) ) ;
#19508 = CARTESIAN_POINT ( 'NONE',  ( 13.11740841389447709, 4.616624901677048420, 5.813473370769506765 ) ) ;
#19509 = LINE ( 'NONE', #14675, #319 ) ;
#19510 = ORIENTED_EDGE ( 'NONE', *, *, #6856, .T. ) ;
#19511 = ORIENTED_EDGE ( 'NONE', *, *, #11563, .F. ) ;
#19512 = LINE ( 'NONE', #19820, #16119 ) ;
#19513 = DIRECTION ( 'NONE',  ( 0.000000000000000000, 0.000000000000000000, 1.000000000000000000 ) ) ;
#19514 = DIRECTION ( 'NONE',  ( 0.000000000000000000, 0.000000000000000000, 1.000000000000000000 ) ) ;
#19515 = DIRECTION ( 'NONE',  ( 1.000000000000000000, 0.000000000000000000, -0.000000000000000000 ) ) ;
#19516 = CARTESIAN_POINT ( 'NONE',  ( 2.282685604506861754, -11.80366834561962364, 2.120553820834011116 ) ) ;
#19517 = DIRECTION ( 'NONE',  ( 0.000000000000000000, 1.000000000000000000, 0.000000000000000000 ) ) ;
#19518 = LINE ( 'NONE', #17930, #11737 ) ;
#19519 = DIRECTION ( 'NONE',  ( 0.1736481776669295540, 0.9848077530122082424, 0.000000000000000000 ) ) ;
#19520 = CARTESIAN_POINT ( 'NONE',  ( 0.000000000000000000, 9.000000000000001776, 0.000000000000000000 ) ) ;
#19521 = CARTESIAN_POINT ( 'NONE',  ( -8.965308582316794173, -20.22900456129164937, 4.174186261275266929 ) ) ;
#19522 = CARTESIAN_POINT ( 'NONE',  ( -1.513434189748285918, -8.364917468222230923, 2.372643865078341019 ) ) ;
#19523 = EDGE_LOOP ( 'NONE', ( #9737, #10028, #5861, #14622 ) ) ;
#19524 = CARTESIAN_POINT ( 'NONE',  ( -12.62958809053144549, -19.26830142816300295, 4.757073430686623361 ) ) ;
#19525 = CARTESIAN_POINT ( 'NONE',  ( -4.840308582316795061, -22.36352608949544418, 4.520995438708343528 ) ) ;
#19526 = EDGE_CURVE ( 'NONE', #734, #458, #20297, .T. ) ;
#19527 = CARTESIAN_POINT ( 'NONE',  ( -7.003441417683177406, -22.05068747287765873, 5.250000000000000888 ) ) ;
#19528 = ORIENTED_EDGE ( 'NONE', *, *, #9473, .F. ) ;
#19529 = ADVANCED_FACE ( 'NONE', ( #18620 ), #7629, .T. ) ;
#19530 = CARTESIAN_POINT ( 'NONE',  ( 13.82092246150448211, 3.019084305971233562, 5.221833296715730377 ) ) ;
#19531 = DIRECTION ( 'NONE',  ( 0.000000000000000000, 0.000000000000000000, -1.000000000000000000 ) ) ;
#19532 = ORIENTED_EDGE ( 'NONE', *, *, #13362, .T. ) ;
#19533 = VERTEX_POINT ( 'NONE', #12229 ) ;
#19534 = PLANE ( 'NONE',  #3714 ) ;
#19535 = ORIENTED_EDGE ( 'NONE', *, *, #5330, .T. ) ;
#19536 = DIRECTION ( 'NONE',  ( 0.000000000000000000, -0.000000000000000000, 1.000000000000000000 ) ) ;
#19537 = ORIENTED_EDGE ( 'NONE', *, *, #13497, .T. ) ;
#19538 = DIRECTION ( 'NONE',  ( -0.000000000000000000, -0.000000000000000000, -1.000000000000000000 ) ) ;
#19539 = EDGE_CURVE ( 'NONE', #11657, #4418, #7991, .T. ) ;
#19540 = DIRECTION ( 'NONE',  ( -4.625929269271477434E-15, -1.000000000000000000, 0.000000000000000000 ) ) ;
#19541 = CARTESIAN_POINT ( 'NONE',  ( -11.00000000000000000, -25.49999999999999645, 4.000000000000000000 ) ) ;
#19542 = DIRECTION ( 'NONE',  ( 1.000000000000000000, 0.000000000000000000, 0.000000000000000000 ) ) ;
#19543 = DIRECTION ( 'NONE',  ( 1.000000000000000000, 0.000000000000000000, 0.000000000000000000 ) ) ;
#19544 = AXIS2_PLACEMENT_3D ( 'NONE', #16410, #16714, #14936 ) ;
#19545 = CARTESIAN_POINT ( 'NONE',  ( 11.22219141768317741, -20.27099543870833998, 4.275561207030583510 ) ) ;
#19546 = CARTESIAN_POINT ( 'NONE',  ( -20.00000000000000000, -0.5000000000000004441, 1.000000000000000000 ) ) ;
#19547 = CARTESIAN_POINT ( 'NONE',  ( -9.909691417683175629, -21.63647391050456648, 4.520995438708348857 ) ) ;
#19548 = VERTEX_POINT ( 'NONE', #10777 ) ;
#19549 = CARTESIAN_POINT ( 'NONE',  ( 8.590308582316797725, -21.01515356694490322, 0.9790045612916562501 ) ) ;
#19550 = CARTESIAN_POINT ( 'NONE',  ( 13.09892531043291086, 3.683228176858501790, 6.000681092915118420 ) ) ;
#19551 = CARTESIAN_POINT ( 'NONE',  ( -12.63249216759192350, -19.87164553660301536, 5.297612231341934041 ) ) ;
#19552 = ORIENTED_EDGE ( 'NONE', *, *, #3626, .F. ) ;
#19553 = DIRECTION ( 'NONE',  ( -0.000000000000000000, -1.000000000000000000, -0.000000000000000000 ) ) ;
#19554 = CARTESIAN_POINT ( 'NONE',  ( 8.119520639128047890, 4.999999999999999112, 1.000000000000000000 ) ) ;
#19555 = ORIENTED_EDGE ( 'NONE', *, *, #6908, .T. ) ;
#19556 = SHAPE_DEFINITION_REPRESENTATION ( #1328, #537 ) ;
#19557 = ORIENTED_EDGE ( 'NONE', *, *, #12309, .F. ) ;
#19558 = DIRECTION ( 'NONE',  ( 1.000000000000000000, 0.000000000000000000, 0.000000000000000000 ) ) ;
#19559 = AXIS2_PLACEMENT_3D ( 'NONE', #19491, #10935, #9467 ) ;
#19560 = ORIENTED_EDGE ( 'NONE', *, *, #2699, .F. ) ;
#19561 = CARTESIAN_POINT ( 'NONE',  ( 13.50000000000000178, 5.000000000000047962, 2.000000000000000000 ) ) ;
#19562 = ADVANCED_FACE ( 'NONE', ( #1460 ), #18831, .F. ) ;
#19563 = CARTESIAN_POINT ( 'NONE',  ( 13.12529397354238192, 5.014845663890295846, 4.666666666666619889 ) ) ;
#19564 = FACE_OUTER_BOUND ( 'NONE', #17139, .T. ) ;
#19565 = AXIS2_PLACEMENT_3D ( 'NONE', #4144, #7497, #4556 ) ;
#19566 = CARTESIAN_POINT ( 'NONE',  ( 12.63249216759192350, -19.87164553660301536, 5.297612231341934041 ) ) ;
#19567 = FACE_OUTER_BOUND ( 'NONE', #19229, .T. ) ;
#19568 = CARTESIAN_POINT ( 'NONE',  ( -13.37524505148396514, -20.23762490005974968, 4.659512268729234741 ) ) ;
#19569 = CARTESIAN_POINT ( 'NONE',  ( 9.059058582316795949, -20.19639159124062999, 5.231925497173373074 ) ) ;
#19570 = CARTESIAN_POINT ( 'NONE',  ( -13.11704875914858270, 3.848462337001107070, 6.754267079155989784 ) ) ;
#19571 = CARTESIAN_POINT ( 'NONE',  ( -5.684058582316795949, -20.26807450282662160, 1.696391591240633101 ) ) ;
#19572 = CARTESIAN_POINT ( 'NONE',  ( -13.81494360078803396, 0.000000000000000000, 1.000000000000000000 ) ) ;
#19573 = DIRECTION ( 'NONE',  ( -0.000000000000000000, -0.000000000000000000, -1.000000000000000000 ) ) ;
#19574 = CARTESIAN_POINT ( 'NONE',  ( 8.777808582316797725, -21.02099543870833998, 3.035098964749253003 ) ) ;
#19575 = CARTESIAN_POINT ( 'NONE',  ( -8.315941417683177406, -20.79840458871654363, 4.773278322869464851 ) ) ;
#19576 = VERTEX_POINT ( 'NONE', #4589 ) ;
#19577 = ORIENTED_EDGE ( 'NONE', *, *, #18571, .T. ) ;
#19578 = CARTESIAN_POINT ( 'NONE',  ( 13.79214722387705905, 1.565934805775630601, 5.190583296715636230 ) ) ;
#19579 = DIRECTION ( 'NONE',  ( -0.000000000000000000, -0.000000000000000000, -1.000000000000000000 ) ) ;
#19580 = ORIENTED_EDGE ( 'NONE', *, *, #5958, .F. ) ;
#19581 = CARTESIAN_POINT ( 'NONE',  ( -14.99999999999998046, -26.49999999999999645, 4.000000000000000000 ) ) ;
#19582 = DIRECTION ( 'NONE',  ( 0.000000000000000000, 1.000000000000000000, -0.000000000000000000 ) ) ;
#19583 = CARTESIAN_POINT ( 'NONE',  ( 0.000000000000000000, 4.999999999999999112, 0.000000000000000000 ) ) ;
#19584 = CARTESIAN_POINT ( 'NONE',  ( 13.39482594849551944, -19.24878960097397140, 5.493002502378098839 ) ) ;
#19585 = FACE_BOUND ( 'NONE', #20441, .T. ) ;
#19586 = CARTESIAN_POINT ( 'NONE',  ( 1.513434189748285696, -9.114917468222230923, 2.372643865078341019 ) ) ;
#19587 = VECTOR ( 'NONE', #6676, 1000.000000000000000 ) ;
#19588 = ADVANCED_FACE ( 'NONE', ( #7839 ), #4394, .T. ) ;
#19589 = DIRECTION ( 'NONE',  ( 0.000000000000000000, -1.000000000000000000, 0.000000000000000000 ) ) ;
#19590 = CARTESIAN_POINT ( 'NONE',  ( -12.70672377255832686, -15.37294948583620346, 4.840845106674187548 ) ) ;
#19591 = CARTESIAN_POINT ( 'NONE',  ( 7.184058582316794173, -20.79840458871652942, 2.226721677130544030 ) ) ;
#19592 = DIRECTION ( 'NONE',  ( 0.000000000000000000, 0.000000000000000000, -1.000000000000000000 ) ) ;
#19593 = CARTESIAN_POINT ( 'NONE',  ( 12.64571531779736979, -19.20387645123237164, 5.508493592915143289 ) ) ;
#19594 = CARTESIAN_POINT ( 'NONE',  ( -1.797604806073912709, -9.120796646272857799, 2.374153755450133740 ) ) ;
#19595 = EDGE_CURVE ( 'NONE', #12236, #12047, #2719, .T. ) ;
#19596 = CARTESIAN_POINT ( 'NONE',  ( 7.277808582316795061, -21.02099543870833998, 3.035098964749253003 ) ) ;
#19597 = ADVANCED_FACE ( 'NONE', ( #6069 ), #12437, .T. ) ;
#19598 = CARTESIAN_POINT ( 'NONE',  ( 11.22219141768317741, -20.27099543870833998, 4.275561207030583510 ) ) ;
#19599 = CARTESIAN_POINT ( 'NONE',  ( -9.715308582316795949, -23.02099543870833998, 3.136473910504556262 ) ) ;
#19600 = VERTEX_POINT ( 'NONE', #6579 ) ;
#19601 = CARTESIAN_POINT ( 'NONE',  ( 13.90439735423812273, 5.734566389025032684, 4.333333333333380999 ) ) ;
#19602 = CARTESIAN_POINT ( 'NONE',  ( 12.64511805349267526, -19.23403829861753422, 5.507852591554869726 ) ) ;
#19603 = CARTESIAN_POINT ( 'NONE',  ( 19.19064177244175440, 0.000000000000000000, 1.000000000000000000 ) ) ;
#19604 = ORIENTED_EDGE ( 'NONE', *, *, #4886, .F. ) ;
#19605 = ORIENTED_EDGE ( 'NONE', *, *, #18332, .T. ) ;
#19606 = CARTESIAN_POINT ( 'NONE',  ( -15.87779268661489773, 10.00000000000000000, 1.000000000000000000 ) ) ;
#19607 = CARTESIAN_POINT ( 'NONE',  ( 24.50000000000000000, 3.000000000000000888, 1.000000000000000000 ) ) ;
#19608 = LINE ( 'NONE', #5263, #20676 ) ;
#19609 = EDGE_CURVE ( 'NONE', #11516, #4449, #19146, .T. ) ;
#19610 = CARTESIAN_POINT ( 'NONE',  ( 14.49999999999998579, -24.47992105705875332, 12.00000000000000000 ) ) ;
#19611 = CARTESIAN_POINT ( 'NONE',  ( 1.776440835594205847, -9.874406767442327038, 1.625080906685880233 ) ) ;
#19612 = CARTESIAN_POINT ( 'NONE',  ( -0.000000000000000000, 10.00000000000000000, 0.000000000000000000 ) ) ;
#19613 = LINE ( 'NONE', #2035, #4724 ) ;
#19614 = CARTESIAN_POINT ( 'NONE',  ( -11.75209451496117197, 11.64110105645932691, 10.00000000000000000 ) ) ;
#19615 = CARTESIAN_POINT ( 'NONE',  ( -2.579281110863027582, -9.822567596814183233, 2.554382554832406615 ) ) ;
#19616 = CARTESIAN_POINT ( 'NONE',  ( -6.434058582316794173, -23.20159541128345992, 4.773278322869455970 ) ) ;
#19617 = CARTESIAN_POINT ( 'NONE',  ( -1.787053415088318609, -8.367039355952382351, 2.373188808236395886 ) ) ;
#19618 = ORIENTED_EDGE ( 'NONE', *, *, #14349, .F. ) ;
#19619 = CARTESIAN_POINT ( 'NONE',  ( -12.89855869007488209, -5.685286151195387383, 5.049178440009032265 ) ) ;
#19620 = CARTESIAN_POINT ( 'NONE',  ( -6.246558582316794173, -21.94931252712234482, 5.250000000000000888 ) ) ;
#19621 = CARTESIAN_POINT ( 'NONE',  ( -9.815941417683177406, -20.79840458871654363, 4.773278322869464851 ) ) ;
#19622 = ORIENTED_EDGE ( 'NONE', *, *, #949, .F. ) ;
#19623 = CARTESIAN_POINT ( 'NONE',  ( 13.84402619238587206, 4.185822715484293077, 5.150938132831436533 ) ) ;
#19624 = CARTESIAN_POINT ( 'NONE',  ( -9.305650798910056309, 9.000000000000001776, 1.000000000000000000 ) ) ;
#19625 = VERTEX_POINT ( 'NONE', #15981 ) ;
#19626 = EDGE_CURVE ( 'NONE', #9770, #10279, #17968, .T. ) ;
#19627 = ORIENTED_EDGE ( 'NONE', *, *, #4292, .F. ) ;
#19628 = CARTESIAN_POINT ( 'NONE',  ( -22.85856191738413656, 0.000000000000000000, 0.000000000000000000 ) ) ;
#19629 = ORIENTED_EDGE ( 'NONE', *, *, #18622, .F. ) ;
#19630 = CARTESIAN_POINT ( 'NONE',  ( -13.39542766346049518, -19.21840299524461315, 5.493648449623241170 ) ) ;
#19631 = ORIENTED_EDGE ( 'NONE', *, *, #12096, .T. ) ;
#19632 = CARTESIAN_POINT ( 'NONE',  ( 6.722191417683176518, -20.27099543870833998, 4.275561207030583510 ) ) ;
#19633 = CARTESIAN_POINT ( 'NONE',  ( -15.61404127825609223, 9.000000000000001776, 0.000000000000000000 ) ) ;
#19634 = EDGE_CURVE ( 'NONE', #10100, #8356, #6483, .T. ) ;
#19635 = EDGE_CURVE ( 'NONE', #15500, #4847, #11491, .T. ) ;
#19636 = CARTESIAN_POINT ( 'NONE',  ( -32.65117217603048516, 6.460468870412185538, 1.000000000000000000 ) ) ;
#19637 = DIRECTION ( 'NONE',  ( 1.000000000000000000, 0.000000000000000000, 0.000000000000000000 ) ) ;
#19638 = CARTESIAN_POINT ( 'NONE',  ( -5.496558582316794173, -22.05068747287764452, 1.749999999999998446 ) ) ;
#19639 = EDGE_CURVE ( 'NONE', #8046, #3441, #196, .T. ) ;
#19640 = FACE_OUTER_BOUND ( 'NONE', #16352, .T. ) ;
#19641 = CARTESIAN_POINT ( 'NONE',  ( 8.972191417683177406, -23.72900456129165292, 2.724438792969417822 ) ) ;
#19642 = LINE ( 'NONE', #8548, #1539 ) ;
#19643 = CARTESIAN_POINT ( 'NONE',  ( -6.253441417683175629, -21.94931252712233061, 2.499999999999999112 ) ) ;
#19644 = CARTESIAN_POINT ( 'NONE',  ( -8.590308582316797725, -21.01515356694490322, 0.9790045612916562501 ) ) ;
#19645 = VERTEX_POINT ( 'NONE', #3540 ) ;
#19646 = CARTESIAN_POINT ( 'NONE',  ( 12.63943061533661982, -19.52125392549825733, 5.470334935344855154 ) ) ;
#19647 = CARTESIAN_POINT ( 'NONE',  ( -13.15498530132288479, 5.764257716805535559, 4.666666666666618113 ) ) ;
#19648 = VERTEX_POINT ( 'NONE', #19554 ) ;
#19649 = EDGE_CURVE ( 'NONE', #2750, #17639, #2675, .T. ) ;
#19650 = DIRECTION ( 'NONE',  ( 0.000000000000000000, 1.000000000000000000, -0.000000000000000000 ) ) ;
#19651 = CARTESIAN_POINT ( 'NONE',  ( -17.05017143803810242, 0.000000000000000000, 0.000000000000000000 ) ) ;
#19652 = ORIENTED_EDGE ( 'NONE', *, *, #12135, .F. ) ;
#19653 = ORIENTED_EDGE ( 'NONE', *, *, #15426, .T. ) ;
#19654 = CARTESIAN_POINT ( 'NONE',  ( 1.811130159782011528, 9.000000000000001776, 0.000000000000000000 ) ) ;
#19655 = ORIENTED_EDGE ( 'NONE', *, *, #14331, .F. ) ;
#19656 = DIRECTION ( 'NONE',  ( -1.000000000000000000, 0.000000000000000000, 0.000000000000000000 ) ) ;
#19657 = CARTESIAN_POINT ( 'NONE',  ( 13.10192273101908000, 3.834597916462216816, 6.003936301248457674 ) ) ;
#19658 = VECTOR ( 'NONE', #7287, 1000.000000000000000 ) ;
#19659 = CARTESIAN_POINT ( 'NONE',  ( 0.000000000000000000, -9.114917468222230923, 2.372643865078340575 ) ) ;
#19660 = CARTESIAN_POINT ( 'NONE',  ( -2.061130159782011972, 9.000000000000001776, 1.000000000000000000 ) ) ;
#19661 = VECTOR ( 'NONE', #19543, 1000.000000000000000 ) ;
#19662 = SHAPE_REPRESENTATION ( 'Fixed Lower Stainless Steel Comb Blade', ( #18039 ), #5348 ) ;
#19663 = CARTESIAN_POINT ( 'NONE',  ( 13.15498530131898214, 5.764257716805535559, 3.333333333333075466 ) ) ;
#19664 = DIRECTION ( 'NONE',  ( -1.000000000000000000, 0.000000000000000000, 0.000000000000000000 ) ) ;
#19665 = CARTESIAN_POINT ( 'NONE',  ( 8.402808582316797725, -23.08622137881038938, 1.020995438708339309 ) ) ;
#19666 = CARTESIAN_POINT ( 'NONE',  ( -13.15492785973632017, 5.761356916681801721, 5.116543252045025802 ) ) ;
#19667 = CARTESIAN_POINT ( 'NONE',  ( -11.78469141768317741, -24.52099543870834708, 4.484846433055073689 ) ) ;
#19668 = DIRECTION ( 'NONE',  ( -1.000000000000000000, -0.000000000000000000, -0.000000000000000000 ) ) ;
#19669 = LINE ( 'NONE', #5334, #17764 ) ;
#19670 = EDGE_CURVE ( 'NONE', #11975, #7606, #1662, .T. ) ;
#19671 = CARTESIAN_POINT ( 'NONE',  ( 11.12155858231679595, -22.99999999999999645, 3.550687472877652073 ) ) ;
#19672 = LINE ( 'NONE', #2605, #2643 ) ;
#19673 = VECTOR ( 'NONE', #11347, 1000.000000000000000 ) ;
#19674 = EDGE_LOOP ( 'NONE', ( #1389, #15592, #2774, #7172 ) ) ;
#19675 = EDGE_LOOP ( 'NONE', ( #3107, #10152, #4258, #8483 ) ) ;
#19676 = CARTESIAN_POINT ( 'NONE',  ( 13.84264281492353987, 3.365962153638767607, 5.979325532956542233 ) ) ;
#19677 = LINE ( 'NONE', #8383, #7148 ) ;
#19678 = PLANE ( 'NONE',  #4016 ) ;
#19679 = VERTEX_POINT ( 'NONE', #405 ) ;
#19680 = CARTESIAN_POINT ( 'NONE',  ( 4.000000000000000000, -8.500000000000000000, 2.392927049865408495 ) ) ;
#19681 = DIRECTION ( 'NONE',  ( -0.000000000000000000, 1.000000000000000000, -0.000000000000000000 ) ) ;
#19682 = LINE ( 'NONE', #5238, #6638 ) ;
#19683 = CARTESIAN_POINT ( 'NONE',  ( 13.85223456079946303, 3.850345320370711644, 5.989742199623227847 ) ) ;
#19684 = AXIS2_PLACEMENT_3D ( 'NONE', #10964, #9394, #8033 ) ;
#19685 = VECTOR ( 'NONE', #466, 1000.000000000000000 ) ;
#19686 = PLANE ( 'NONE',  #1513 ) ;
#19687 = CARTESIAN_POINT ( 'NONE',  ( 3.302240162463773832, -9.695145533921818881, 2.714273006325518711 ) ) ;
#19688 = AXIS2_PLACEMENT_3D ( 'NONE', #13584, #19985, #2499 ) ;
#19689 = CARTESIAN_POINT ( 'NONE',  ( -9.689245429134309973, 10.00000000000000000, 0.000000000000000000 ) ) ;
#19690 = CARTESIAN_POINT ( 'NONE',  ( -12.99447614883396973, -0.8414544838704021146, 5.153345106674984244 ) ) ;
#19691 = CARTESIAN_POINT ( 'NONE',  ( 8.027808582316792396, -23.72900456129165292, 4.275561207030568411 ) ) ;
#19692 = LINE ( 'NONE', #2738, #2057 ) ;
#19693 = CARTESIAN_POINT ( 'NONE',  ( 12.64131715375063258, -19.42598373559290792, 5.491151580003103660 ) ) ;
#19694 = CARTESIAN_POINT ( 'NONE',  ( -1.407845757905374695, -9.864917468222230923, 2.372643865078341019 ) ) ;
#19695 = VECTOR ( 'NONE', #10103, 1000.000000000000000 ) ;
#19696 = CARTESIAN_POINT ( 'NONE',  ( 12.52780858231679773, -22.97900456129165647, 3.964901035250747885 ) ) ;
#19697 = CARTESIAN_POINT ( 'NONE',  ( 11.12844141768317741, -20.24999999999999289, 3.550687472877664952 ) ) ;
#19698 = CARTESIAN_POINT ( 'NONE',  ( -6.434058582316796837, -22.67126532539354855, 4.242948236979545484 ) ) ;
#19699 = ORIENTED_EDGE ( 'NONE', *, *, #197, .T. ) ;
#19700 = CARTESIAN_POINT ( 'NONE',  ( 12.96597876160390683, -3.780572539034193102, 6.590204579154564257 ) ) ;
#19701 = CARTESIAN_POINT ( 'NONE',  ( 12.62837453896009876, -19.32958578251692572, 4.742959489302074338 ) ) ;
#19702 = VECTOR ( 'NONE', #5606, 1000.000000000000000 ) ;
#19703 = CARTESIAN_POINT ( 'NONE',  ( -12.80505314591509070, -19.91502843109724097, 3.526594361829830326 ) ) ;
#19704 = VERTEX_POINT ( 'NONE', #4801 ) ;
#19705 = EDGE_CURVE ( 'NONE', #962, #2639, #20712, .T. ) ;
#19706 = AXIS2_PLACEMENT_3D ( 'NONE', #3898, #5680, #20123 ) ;
#19707 = ORIENTED_EDGE ( 'NONE', *, *, #5615, .T. ) ;
#19708 = DIRECTION ( 'NONE',  ( 1.000000000000000000, 0.000000000000000000, 0.000000000000000000 ) ) ;
#19709 = VECTOR ( 'NONE', #15638, 1000.000000000000000 ) ;
#19710 = AXIS2_PLACEMENT_3D ( 'NONE', #16414, #2089, #19468 ) ;
#19711 = CARTESIAN_POINT ( 'NONE',  ( 14.50000000000001243, -25.49999999999999645, 4.000000000000000000 ) ) ;
#19712 = ADVANCED_FACE ( 'NONE', ( #5002 ), #8156, .T. ) ;
#19713 = CYLINDRICAL_SURFACE ( 'NONE', #14982, 10.00000000000000000 ) ;
#19714 = CARTESIAN_POINT ( 'NONE',  ( -4.121804964265450621, -21.50709082768453939, 5.525644484121333022 ) ) ;
#19715 = CARTESIAN_POINT ( 'NONE',  ( 0.2815691515810352374, -9.864917468222230923, 2.372643865078523540 ) ) ;
#19716 = PLANE ( 'NONE',  #8396 ) ;
#19717 = DIRECTION ( 'NONE',  ( -1.000000000000000000, -0.000000000000000000, -0.000000000000000000 ) ) ;
#19718 = CARTESIAN_POINT ( 'NONE',  ( 13.26220787538139589, -20.51810926806117763, 3.464229958566896084 ) ) ;
#19719 = COLOUR_RGB ( '', 0.40784314, 0.44705882, 0.49803922) ;
#19720 = DIRECTION ( 'NONE',  ( -1.013672804646636192E-16, 1.000000000000000000, 0.000000000000000000 ) ) ;
#19721 = CARTESIAN_POINT ( 'NONE',  ( -5.496558582316794173, -22.05068747287764452, 1.749999999999998446 ) ) ;
#19722 = CARTESIAN_POINT ( 'NONE',  ( -4.066879903460562495, -13.96783368734915776, 3.061584679647603391 ) ) ;
#19723 = ORIENTED_EDGE ( 'NONE', *, *, #6571, .T. ) ;
#19724 = CARTESIAN_POINT ( 'NONE',  ( -13.68663801924254741, -3.762280028282741551, 5.075999963380942503 ) ) ;
#19725 = CARTESIAN_POINT ( 'NONE',  ( -9.152808582316794173, -21.22443879296942626, 5.229004561291659137 ) ) ;
#19726 = AXIS2_PLACEMENT_3D ( 'NONE', #12876, #1699, #13186 ) ;
#19727 = CARTESIAN_POINT ( 'NONE',  ( -5.222191417683178294, -20.27099543870833998, 4.275561207030583510 ) ) ;
#19728 = ORIENTED_EDGE ( 'NONE', *, *, #11418, .F. ) ;
#19729 = CARTESIAN_POINT ( 'NONE',  ( 13.37500015856764435, -20.24999199233421265, 4.532157119432948633 ) ) ;
#19730 = LINE ( 'NONE', #15311, #5366 ) ;
#19731 = VERTEX_POINT ( 'NONE', #12744 ) ;
#19732 = VERTEX_POINT ( 'NONE', #8050 ) ;
#19733 = DIRECTION ( 'NONE',  ( 0.000000000000000000, 1.000000000000000000, -0.000000000000000000 ) ) ;
#19734 = ADVANCED_FACE ( 'NONE', ( #17556 ), #6788, .F. ) ;
#19735 = ORIENTED_EDGE ( 'NONE', *, *, #10162, .F. ) ;
#19736 = CARTESIAN_POINT ( 'NONE',  ( 9.000000000000000000, -9.999999999999991118, 2.000000000000000000 ) ) ;
#19737 = ORIENTED_EDGE ( 'NONE', *, *, #14456, .T. ) ;
#19738 = EDGE_CURVE ( 'NONE', #610, #20018, #19455, .T. ) ;
#19739 = EDGE_CURVE ( 'NONE', #6837, #10229, #15879, .T. ) ;
#19740 = ORIENTED_EDGE ( 'NONE', *, *, #18198, .T. ) ;
#19741 = CIRCLE ( 'NONE', #17733, 0.3749999999999997224 ) ;
#19742 = CARTESIAN_POINT ( 'NONE',  ( 6.065941417683177406, -23.20159541128344927, 2.226721677130534705 ) ) ;
#19743 = LINE ( 'NONE', #19440, #2977 ) ;
#19744 = VECTOR ( 'NONE', #1222, 1000.000000000000000 ) ;
#19745 = CARTESIAN_POINT ( 'NONE',  ( -20.75349085826862350, 0.000000000000000000, 1.000000000000000000 ) ) ;
#19746 = CARTESIAN_POINT ( 'NONE',  ( 1.407845757905374695, -8.364917468222230923, 2.372643865078341019 ) ) ;
#19747 = CARTESIAN_POINT ( 'NONE',  ( -6.246558582316794173, -21.94931252712234482, 5.250000000000000888 ) ) ;
#19748 = CARTESIAN_POINT ( 'NONE',  ( 13.90439771357353038, 5.734584535470497180, 4.942866369314573127 ) ) ;
#19749 = DIRECTION ( 'NONE',  ( 0.000000000000000000, 1.000000000000000000, -0.000000000000000000 ) ) ;
#19750 = CARTESIAN_POINT ( 'NONE',  ( 11.40969141768317918, -21.63647391050456648, 4.520995438708348857 ) ) ;
#19751 = LINE ( 'NONE', #13454, #13221 ) ;
#19752 = CARTESIAN_POINT ( 'NONE',  ( -8.128441417683177406, -20.99999999999999645, 3.550687472877664952 ) ) ;
#19753 = CARTESIAN_POINT ( 'NONE',  ( -6.621558582316796837, -24.50000000000000000, 3.550687472877651629 ) ) ;
#19754 = ORIENTED_EDGE ( 'NONE', *, *, #11934, .T. ) ;
#19755 = CARTESIAN_POINT ( 'NONE',  ( 12.95145221759166354, -3.764163011652346569, 5.840524842913703552 ) ) ;
#19756 = CARTESIAN_POINT ( 'NONE',  ( -12.62499999999998224, -20.25000000000006395, 4.416666666666681174 ) ) ;
#19757 = ORIENTED_EDGE ( 'NONE', *, *, #1373, .T. ) ;
#19758 = VECTOR ( 'NONE', #19287, 1000.000000000000000 ) ;
#19759 = DIRECTION ( 'NONE',  ( -0.000000000000000000, -0.000000000000000000, -1.000000000000000000 ) ) ;
#19760 = ADVANCED_FACE ( 'NONE', ( #16204 ), #6376, .T. ) ;
#19761 = FACE_OUTER_BOUND ( 'NONE', #15157, .T. ) ;
#19762 = CIRCLE ( 'NONE', #13395, 10.00000000000000000 ) ;
#19763 = EDGE_CURVE ( 'NONE', #20538, #17687, #19247, .T. ) ;
#19764 = ORIENTED_EDGE ( 'NONE', *, *, #13431, .F. ) ;
#19765 = APPLICATION_PROTOCOL_DEFINITION ( 'draft international standard', 'automotive_design', 1998, #131 ) ;
#19766 = VERTEX_POINT ( 'NONE', #4898 ) ;
#19767 = DIRECTION ( 'NONE',  ( 0.000000000000000000, 0.000000000000000000, -1.000000000000000000 ) ) ;
#19768 = ORIENTED_EDGE ( 'NONE', *, *, #13976, .T. ) ;
#19769 = CYLINDRICAL_SURFACE ( 'NONE', #17997, 0.3749999999999997224 ) ;
#19770 = CARTESIAN_POINT ( 'NONE',  ( 13.08573665985359824, 3.017201322601628100, 5.986358176248492313 ) ) ;
#19771 = CARTESIAN_POINT ( 'NONE',  ( -3.232228556578340850, -13.29361487011126464, 2.695816835751057461 ) ) ;
#19772 = CARTESIAN_POINT ( 'NONE',  ( 0.5631383031621635116, -9.114917468222230923, 2.372643865078341019 ) ) ;
#19773 = FACE_BOUND ( 'NONE', #4395, .T. ) ;
#19774 = VECTOR ( 'NONE', #623, 1000.000000000000000 ) ;
#19775 = LINE ( 'NONE', #728, #1400 ) ;
#19776 = CARTESIAN_POINT ( 'NONE',  ( -5.933390479346035029, 9.000000000000001776, 1.000000000000000000 ) ) ;
#19777 = CARTESIAN_POINT ( 'NONE',  ( 12.34030858231679773, -22.98484643305508612, 6.020995438708344416 ) ) ;
#19778 = CARTESIAN_POINT ( 'NONE',  ( -13.07148796623841847, 1.547642295024179493, 6.704787912489258872 ) ) ;
#19779 = CARTESIAN_POINT ( 'NONE',  ( -7.940941417683175629, -20.19639159124061933, 1.768074502826635586 ) ) ;
#19780 = APPLICATION_CONTEXT ( 'automotive_design' ) ;
#19781 = ORIENTED_EDGE ( 'NONE', *, *, #2352, .F. ) ;
#19782 = DIRECTION ( 'NONE',  ( 0.000000000000000000, 0.000000000000000000, 1.000000000000000000 ) ) ;
#19783 = FACE_OUTER_BOUND ( 'NONE', #19041, .T. ) ;
#19784 = CARTESIAN_POINT ( 'NONE',  ( 8.496558582316795949, -22.05068747287764452, 2.499999999999999112 ) ) ;
#19785 = EDGE_CURVE ( 'NONE', #7462, #2297, #8252, .T. ) ;
#19786 = FACE_OUTER_BOUND ( 'NONE', #7992, .T. ) ;
#19787 = ORIENTED_EDGE ( 'NONE', *, *, #570, .T. ) ;
#19788 = EDGE_CURVE ( 'NONE', #9899, #485, #9714, .T. ) ;
#19789 = VERTEX_POINT ( 'NONE', #10333 ) ;
#19790 = CARTESIAN_POINT ( 'NONE',  ( 13.54769662923970763, -11.52882022337116119, 5.659013032956382361 ) ) ;
#19791 = DIRECTION ( 'NONE',  ( 1.000000000000000000, 0.000000000000000000, 0.000000000000000000 ) ) ;
#19792 = DIRECTION ( 'NONE',  ( 1.000000000000000000, 0.000000000000000000, 0.000000000000000000 ) ) ;
#19793 = ORIENTED_EDGE ( 'NONE', *, *, #14762, .F. ) ;
#19794 = VECTOR ( 'NONE', #18988, 1000.000000000000000 ) ;
#19795 = DIRECTION ( 'NONE',  ( -5.204170427930411817E-15, 1.000000000000000000, 0.000000000000000000 ) ) ;
#19796 = CARTESIAN_POINT ( 'NONE',  ( -7.369520639128046113, 4.999999999999999112, 1.000000000000000000 ) ) ;
#19797 = DIRECTION ( 'NONE',  ( 0.000000000000000000, 1.000000000000000000, 0.000000000000000000 ) ) ;
#19798 = CARTESIAN_POINT ( 'NONE',  ( 13.86106797245302147, 4.296432608878145487, 5.947261916831099171 ) ) ;
#19799 =( BOUNDED_SURFACE ( )  B_SPLINE_SURFACE ( 3, 2, ( 
 ( #12349, #15486, #18535, #12244, #15074, #10687, #7239, #17059, #3991, #10375, #755, #7142, #19907, #4198, #13911, #5561, #7344, #16947, #11932, #16749, #13601, #2420, #8811, #9014, #20312, #5669, #5976, #4097, #16850, #15277, #15386, #18746, #13706, #1069, #20528, #19055, #17679, #12454, #12549, #18849, #4818, #3148, #15893, #9215, #12651, #1378, #2937, #12859, #4, #7947, #10894, #9317, #14430, #1678, #7853, #19261, #4603, #9618, #1573, #112, #15586, #17258, #11292, #12759, #14319, #6182, #1270, #15693, #16001, #17471, #7647, #9521, #3244, #6394, #8067, #18947, #10995, #14019, #19162, #7756, #11195, #4510, #17572, #6498, #20427, #4915, #14123, #17364, #3051, #6087, #9426, #15795, #14217, #1476, #20624 ),
 ( #6277, #4712, #11100, #11505, #5020, #10037, #10144, #18099, #5125, #7006, #13169, #19777, #17885, #11400, #13071, #16312, #16515, #19470, #3453, #13374, #3350, #1985, #16415, #8475, #2187, #14745, #9730, #8571, #5435, #17984, #6898, #14631, #19364, #11702, #16114, #11808, #3655, #3764, #8372, #421, #3552, #619, #1782, #8169, #6801, #9932, #19569, #14941, #14535, #210, #17785, #6594, #5222, #19665, #12962, #9831, #13266, #16216, #11600, #14842, #1884, #8265, #316, #5328, #6700, #2090, #517, #18610, #4270, #15045, #10554, #5638, #19977, #12011, #18199, #828, #10239, #3862, #8883, #13887, #18296, #19880, #16605, #5536, #20083, #2597, #8985, #2490, #15252, #9091, #18512, #2395, #10657, #4172, #2709 ),
 ( #13575, #18407, #7523, #5750, #15461, #17031, #13786, #16923, #4071, #15358, #7213, #5851, #20288, #1038, #2285, #5946, #12220, #10457, #8676, #16826, #1146, #928, #7315, #15154, #7114, #7424, #13676, #3959, #730, #13477, #20191, #12120, #11906, #10347, #16719, #8785, #3022, #6251, #6159, #12526, #2814, #20702, #14291, #13988, #4789, #1350, #9188, #7830, #17339, #10767, #9593, #3223, #18923, #17235, #1546, #14192, #3124, #10870, #9499, #7731, #20599, #6365, #14403, #12734, #18823, #15970, #19137, #15770, #15870, #1653, #7925, #4486, #11172, #15563, #1246, #8037, #88, #12319, #1452, #17545, #18717, #4581, #12625, #4384, #17135, #2914, #7619, #20396, #19029, #17446, #6059, #4684, #12429, #9290, #20505 ),
 ( #15665, #14096, #10968, #9398, #11075, #11267, #5299, #6568, #2067, #3531, #12933, #13148, #17861, #14606, #8145, #19545, #13243, #494, #8241, #10119, #16288, #2163, #284, #19237, #14508, #8342, #11578, #17957, #11481, #9906, #18071, #6778, #11372, #8547, #10010, #3629, #17761, #14917, #19338, #19641, #14718, #4887, #395, #6874, #5200, #11674, #9807, #1858, #12834, #16389, #4993, #8452, #16089, #14819, #3737, #17647, #16491, #3430, #186, #16194, #3321, #6675, #13044, #5102, #9703, #6475, #19444, #1759, #1959, #7088, #7289, #11988, #8759, #2261, #13652, #7403, #15332, #2371, #4250, #10432, #17007, #15132, #8650, #10324, #13553, #13764, #16693, #703, #10630, #595, #19954, #20063, #5727, #20168, #18386 ),
 ( #15230, #4149, #11882, #16584, #8957, #13349, #2684, #904, #1012, #5612, #4049, #806, #18587, #19750, #5408, #16801, #7190, #2470, #5828, #9070, #12197, #15022, #6981, #8861, #16901, #10216, #11782, #10532, #18174, #12098, #18488, #3837, #13453, #19857, #2572, #5510, #18274, #3936, #15848, #1527, #12296, #7810, #2892, #17214, #9268, #15442, #18800, #7504, #1126, #6137, #11151, #15544, #17113, #4359, #1429, #4561, #1224, #13867, #20266, #14172, #10946, #18904, #14270, #15747, #3202, #12506, #9373, #15640, #1329, #5925, #3101, #17425, #2795, #7906, #4466, #18693, #17312, #20481, #10743, #12711, #6340, #7705, #20371, #4661, #2997, #6232, #13966, #12602, #10851, #20579, #9478, #17521, #20677, #7599, #19113 ),
 ( #4766, #19005, #6034, #9169, #12406, #14073, #11052, #5564, #18330, #19696, #18227, #9573, #16446, #5359, #15946, #14381, #16065, #64, #6450, #13295, #14970, #19911, #2216, #8008, #12814, #18017, #11736, #8599, #649, #8706, #450, #18129, #1628, #19213, #13198, #4867, #5465, #3794, #16541, #11246, #10171, #1738, #3297, #13509, #7037, #13405, #17625, #9679, #15077, #2317, #8501, #11936, #5249, #10269, #19811, #760, #8120, #14487, #11837, #11627, #3687, #6828, #3890, #7145, #16638, #19596, #10071, #2119, #14871, #547, #6926, #6090, #2741, #10379, #20432, #12355, #16952, #16752, #5778, #2842, #9018, #12148, #958, #10799, #1273, #17166, #20009, #9218, #20115, #20316, #13604, #14023, #13914, #2424, #20217 ),
 ( #5672, #15589, #13709, #860, #5878, #15389, #8815, #7652, #12458, #10584, #8913, #5980, #12248, #15490, #2521, #1173, #18538, #18640, #18749, #3995, #4413, #10484, #15183, #7243, #7453, #7552, #12044, #18437, #16854, #4101, #15281, #7348, #4202, #2630, #1072, #13814, #4306, #10691, #17062, #9121, #4513, #2940, #4606, #9321, #15697, #1577, #3248, #8172, #11201, #17261, #1381, #6281, #10, #17576, #9622, #17684, #9429, #7951, #6599, #7761, #1478, #14127, #14435, #12763, #4822, #18852, #14325, #10999, #12552, #1786, #16006, #1685, #20531, #18951, #3354, #11296, #17476, #14539, #14220, #19267, #8071, #9734, #10898, #6185, #6398, #20627, #12655, #213, #19168, #16118, #4919, #117, #6503, #19058, #12863 ) ),
 .UNSPECIFIED., .T., .F., .T. ) 
 B_SPLINE_SURFACE_WITH_KNOTS ( ( 4, 3, 4 ),
 ( 3, 2, 2, 2, 2, 2, 2, 2, 2, 2, 2, 2, 2, 2, 2, 2, 2, 2, 2, 2, 2, 2, 2, 2, 2, 2, 2, 2, 2, 2, 2, 2, 2, 2, 2, 2, 2, 2, 2, 2, 2, 2, 2, 2, 2, 2, 2, 3 ),
 ( 0.000000000000000000, 0.5000000000000000000, 1.000000000000000000 ),
 ( 0.000000000000000000, 0.02083333333333333218, 0.04166666666666666435, 0.06250000000000000000, 0.08333333333333332871, 0.1041666666666666713, 0.1250000000000000000, 0.1458333333333333426, 0.1666666666666666574, 0.1875000000000000000, 0.2083333333333333426, 0.2291666666666666574, 0.2500000000000000000, 0.2708333333333333148, 0.2916666666666666852, 0.3125000000000000000, 0.3333333333333333148, 0.3541666666666666852, 0.3750000000000000000, 0.3958333333333333148, 0.4166666666666666852, 0.4375000000000000000, 0.4583333333333333148, 0.4791666666666666852, 0.5000000000000000000, 0.5208333333333333703, 0.5416666666666666297, 0.5625000000000000000, 0.5833333333333333703, 0.6041666666666666297, 0.6250000000000000000, 0.6458333333333333703, 0.6666666666666666297, 0.6875000000000000000, 0.7083333333333333703, 0.7291666666666666297, 0.7500000000000000000, 0.7708333333333333703, 0.7916666666666666297, 0.8125000000000000000, 0.8333333333333333703, 0.8541666666666666297, 0.8750000000000000000, 0.8958333333333333703, 0.9166666666666666297, 0.9375000000000000000, 0.9583333333333333703, 0.9650437087885355147 ),
 .UNSPECIFIED. ) 
 GEOMETRIC_REPRESENTATION_ITEM ( )  RATIONAL_B_SPLINE_SURFACE ( (
 ( 1.000000000000000000, 0.9238795325112867385, 1.000000000000000000, 0.9238795325112867385, 1.000000000000000000, 0.9238795325112867385, 1.000000000000000000, 0.9238795325112867385, 1.000000000000000000, 0.9238795325112867385, 1.000000000000000000, 0.9238795325112867385, 1.000000000000000000, 0.9238795325112867385, 1.000000000000000000, 0.9238795325112867385, 1.000000000000000000, 0.9238795325112867385, 1.000000000000000000, 0.9238795325112867385, 1.000000000000000000, 0.9238795325112867385, 1.000000000000000000, 0.9238795325112867385, 1.000000000000000000, 0.9238795325112867385, 1.000000000000000000, 0.9238795325112867385, 1.000000000000000000, 0.9238795325112867385, 1.000000000000000000, 0.9238795325112867385, 1.000000000000000000, 0.9238795325112867385, 1.000000000000000000, 0.9238795325112867385, 1.000000000000000000, 0.9238795325112867385, 1.000000000000000000, 0.9238795325112867385, 1.000000000000000000, 0.9238795325112867385, 1.000000000000000000, 0.9238795325112867385, 1.000000000000000000, 0.9238795325112867385, 1.000000000000000000, 0.9238795325112867385, 1.000000000000000000, 0.9238795325112867385, 1.000000000000000000, 0.9238795325112867385, 1.000000000000000000, 0.9238795325112867385, 1.000000000000000000, 0.9238795325112867385, 1.000000000000000000, 0.9238795325112867385, 1.000000000000000000, 0.9238795325112867385, 1.000000000000000000, 0.9238795325112867385, 1.000000000000000000, 0.9238795325112867385, 1.000000000000000000, 0.9238795325112867385, 1.000000000000000000, 0.9238795325112867385, 1.000000000000000000, 0.9238795325112867385, 1.000000000000000000, 0.9238795325112867385, 1.000000000000000000, 0.9238795325112867385, 1.000000000000000000, 0.9238795325112867385, 1.000000000000000000, 0.9238795325112867385, 1.000000000000000000, 0.9238795325112867385, 1.000000000000000000, 0.9238795325112867385, 1.000000000000000000, 0.9238795325112867385, 1.000000000000000000, 0.9238795325112867385, 1.000000000000000000, 0.9238795325112867385, 1.000000000000000000, 0.9238795325112867385, 1.000000000000000000, 0.9238795325112867385, 1.000000000000000000, 0.9754817479996107377, 0.9667580569362973497),
 ( 0.3333333333333333703, 0.3079598441704289313, 0.3333333333333333703, 0.3079598441704289313, 0.3333333333333333703, 0.3079598441704289313, 0.3333333333333333703, 0.3079598441704289313, 0.3333333333333333703, 0.3079598441704289313, 0.3333333333333333703, 0.3079598441704289313, 0.3333333333333333703, 0.3079598441704289313, 0.3333333333333333703, 0.3079598441704289313, 0.3333333333333333703, 0.3079598441704289313, 0.3333333333333333703, 0.3079598441704289313, 0.3333333333333333703, 0.3079598441704289313, 0.3333333333333333703, 0.3079598441704289313, 0.3333333333333333703, 0.3079598441704289313, 0.3333333333333333703, 0.3079598441704289313, 0.3333333333333333703, 0.3079598441704289313, 0.3333333333333333703, 0.3079598441704289313, 0.3333333333333333703, 0.3079598441704289313, 0.3333333333333333703, 0.3079598441704289313, 0.3333333333333333703, 0.3079598441704289313, 0.3333333333333333703, 0.3079598441704289313, 0.3333333333333333703, 0.3079598441704289313, 0.3333333333333333703, 0.3079598441704289313, 0.3333333333333333703, 0.3079598441704289313, 0.3333333333333333703, 0.3079598441704289313, 0.3333333333333333703, 0.3079598441704289313, 0.3333333333333333703, 0.3079598441704289313, 0.3333333333333333703, 0.3079598441704289313, 0.3333333333333333703, 0.3079598441704289313, 0.3333333333333333703, 0.3079598441704289313, 0.3333333333333333703, 0.3079598441704289313, 0.3333333333333333703, 0.3079598441704289313, 0.3333333333333333703, 0.3079598441704289313, 0.3333333333333333703, 0.3079598441704289313, 0.3333333333333333703, 0.3079598441704289313, 0.3333333333333333703, 0.3079598441704289313, 0.3333333333333333703, 0.3079598441704289313, 0.3333333333333333703, 0.3079598441704289313, 0.3333333333333333703, 0.3079598441704289313, 0.3333333333333333703, 0.3079598441704289313, 0.3333333333333333703, 0.3079598441704289313, 0.3333333333333333703, 0.3079598441704289313, 0.3333333333333333703, 0.3079598441704289313, 0.3333333333333333703, 0.3079598441704289313, 0.3333333333333333703, 0.3079598441704289313, 0.3333333333333333703, 0.3079598441704289313, 0.3333333333333333703, 0.3079598441704289313, 0.3333333333333333703, 0.3251605826665369681, 0.3222526856454325239),
 ( 0.3333333333333333703, 0.3079598441704289313, 0.3333333333333333703, 0.3079598441704289313, 0.3333333333333333703, 0.3079598441704289313, 0.3333333333333333703, 0.3079598441704289313, 0.3333333333333333703, 0.3079598441704289313, 0.3333333333333333703, 0.3079598441704289313, 0.3333333333333333703, 0.3079598441704289313, 0.3333333333333333703, 0.3079598441704289313, 0.3333333333333333703, 0.3079598441704289313, 0.3333333333333333703, 0.3079598441704289313, 0.3333333333333333703, 0.3079598441704289313, 0.3333333333333333703, 0.3079598441704289313, 0.3333333333333333703, 0.3079598441704289313, 0.3333333333333333703, 0.3079598441704289313, 0.3333333333333333703, 0.3079598441704289313, 0.3333333333333333703, 0.3079598441704289313, 0.3333333333333333703, 0.3079598441704289313, 0.3333333333333333703, 0.3079598441704289313, 0.3333333333333333703, 0.3079598441704289313, 0.3333333333333333703, 0.3079598441704289313, 0.3333333333333333703, 0.3079598441704289313, 0.3333333333333333703, 0.3079598441704289313, 0.3333333333333333703, 0.3079598441704289313, 0.3333333333333333703, 0.3079598441704289313, 0.3333333333333333703, 0.3079598441704289313, 0.3333333333333333703, 0.3079598441704289313, 0.3333333333333333703, 0.3079598441704289313, 0.3333333333333333703, 0.3079598441704289313, 0.3333333333333333703, 0.3079598441704289313, 0.3333333333333333703, 0.3079598441704289313, 0.3333333333333333703, 0.3079598441704289313, 0.3333333333333333703, 0.3079598441704289313, 0.3333333333333333703, 0.3079598441704289313, 0.3333333333333333703, 0.3079598441704289313, 0.3333333333333333703, 0.3079598441704289313, 0.3333333333333333703, 0.3079598441704289313, 0.3333333333333333703, 0.3079598441704289313, 0.3333333333333333703, 0.3079598441704289313, 0.3333333333333333703, 0.3079598441704289313, 0.3333333333333333703, 0.3079598441704289313, 0.3333333333333333703, 0.3079598441704289313, 0.3333333333333333703, 0.3079598441704289313, 0.3333333333333333703, 0.3079598441704289313, 0.3333333333333333703, 0.3079598441704289313, 0.3333333333333333703, 0.3079598441704289313, 0.3333333333333333703, 0.3079598441704289313, 0.3333333333333333703, 0.3251605826665369681, 0.3222526856454325239),
 ( 1.000000000000000000, 0.9238795325112867385, 1.000000000000000000, 0.9238795325112867385, 1.000000000000000000, 0.9238795325112867385, 1.000000000000000000, 0.9238795325112867385, 1.000000000000000000, 0.9238795325112867385, 1.000000000000000000, 0.9238795325112867385, 1.000000000000000000, 0.9238795325112867385, 1.000000000000000000, 0.9238795325112867385, 1.000000000000000000, 0.9238795325112867385, 1.000000000000000000, 0.9238795325112867385, 1.000000000000000000, 0.9238795325112867385, 1.000000000000000000, 0.9238795325112867385, 1.000000000000000000, 0.9238795325112867385, 1.000000000000000000, 0.9238795325112867385, 1.000000000000000000, 0.9238795325112867385, 1.000000000000000000, 0.9238795325112867385, 1.000000000000000000, 0.9238795325112867385, 1.000000000000000000, 0.9238795325112867385, 1.000000000000000000, 0.9238795325112867385, 1.000000000000000000, 0.9238795325112867385, 1.000000000000000000, 0.9238795325112867385, 1.000000000000000000, 0.9238795325112867385, 1.000000000000000000, 0.9238795325112867385, 1.000000000000000000, 0.9238795325112867385, 1.000000000000000000, 0.9238795325112867385, 1.000000000000000000, 0.9238795325112867385, 1.000000000000000000, 0.9238795325112867385, 1.000000000000000000, 0.9238795325112867385, 1.000000000000000000, 0.9238795325112867385, 1.000000000000000000, 0.9238795325112867385, 1.000000000000000000, 0.9238795325112867385, 1.000000000000000000, 0.9238795325112867385, 1.000000000000000000, 0.9238795325112867385, 1.000000000000000000, 0.9238795325112867385, 1.000000000000000000, 0.9238795325112867385, 1.000000000000000000, 0.9238795325112867385, 1.000000000000000000, 0.9238795325112867385, 1.000000000000000000, 0.9238795325112867385, 1.000000000000000000, 0.9238795325112867385, 1.000000000000000000, 0.9238795325112867385, 1.000000000000000000, 0.9238795325112867385, 1.000000000000000000, 0.9238795325112867385, 1.000000000000000000, 0.9238795325112867385, 1.000000000000000000, 0.9238795325112867385, 1.000000000000000000, 0.9238795325112867385, 1.000000000000000000, 0.9238795325112867385, 1.000000000000000000, 0.9754817479996107377, 0.9667580569362973497),
 ( 0.3333333333333333703, 0.3079598441704289313, 0.3333333333333333703, 0.3079598441704289313, 0.3333333333333333703, 0.3079598441704289313, 0.3333333333333333703, 0.3079598441704289313, 0.3333333333333333703, 0.3079598441704289313, 0.3333333333333333703, 0.3079598441704289313, 0.3333333333333333703, 0.3079598441704289313, 0.3333333333333333703, 0.3079598441704289313, 0.3333333333333333703, 0.3079598441704289313, 0.3333333333333333703, 0.3079598441704289313, 0.3333333333333333703, 0.3079598441704289313, 0.3333333333333333703, 0.3079598441704289313, 0.3333333333333333703, 0.3079598441704289313, 0.3333333333333333703, 0.3079598441704289313, 0.3333333333333333703, 0.3079598441704289313, 0.3333333333333333703, 0.3079598441704289313, 0.3333333333333333703, 0.3079598441704289313, 0.3333333333333333703, 0.3079598441704289313, 0.3333333333333333703, 0.3079598441704289313, 0.3333333333333333703, 0.3079598441704289313, 0.3333333333333333703, 0.3079598441704289313, 0.3333333333333333703, 0.3079598441704289313, 0.3333333333333333703, 0.3079598441704289313, 0.3333333333333333703, 0.3079598441704289313, 0.3333333333333333703, 0.3079598441704289313, 0.3333333333333333703, 0.3079598441704289313, 0.3333333333333333703, 0.3079598441704289313, 0.3333333333333333703, 0.3079598441704289313, 0.3333333333333333703, 0.3079598441704289313, 0.3333333333333333703, 0.3079598441704289313, 0.3333333333333333703, 0.3079598441704289313, 0.3333333333333333703, 0.3079598441704289313, 0.3333333333333333703, 0.3079598441704289313, 0.3333333333333333703, 0.3079598441704289313, 0.3333333333333333703, 0.3079598441704289313, 0.3333333333333333703, 0.3079598441704289313, 0.3333333333333333703, 0.3079598441704289313, 0.3333333333333333703, 0.3079598441704289313, 0.3333333333333333703, 0.3079598441704289313, 0.3333333333333333703, 0.3079598441704289313, 0.3333333333333333703, 0.3079598441704289313, 0.3333333333333333703, 0.3079598441704289313, 0.3333333333333333703, 0.3079598441704289313, 0.3333333333333333703, 0.3079598441704289313, 0.3333333333333333703, 0.3079598441704289313, 0.3333333333333333703, 0.3079598441704289313, 0.3333333333333333703, 0.3251605826665369681, 0.3222526856454325239),
 ( 0.3333333333333333703, 0.3079598441704289313, 0.3333333333333333703, 0.3079598441704289313, 0.3333333333333333703, 0.3079598441704289313, 0.3333333333333333703, 0.3079598441704289313, 0.3333333333333333703, 0.3079598441704289313, 0.3333333333333333703, 0.3079598441704289313, 0.3333333333333333703, 0.3079598441704289313, 0.3333333333333333703, 0.3079598441704289313, 0.3333333333333333703, 0.3079598441704289313, 0.3333333333333333703, 0.3079598441704289313, 0.3333333333333333703, 0.3079598441704289313, 0.3333333333333333703, 0.3079598441704289313, 0.3333333333333333703, 0.3079598441704289313, 0.3333333333333333703, 0.3079598441704289313, 0.3333333333333333703, 0.3079598441704289313, 0.3333333333333333703, 0.3079598441704289313, 0.3333333333333333703, 0.3079598441704289313, 0.3333333333333333703, 0.3079598441704289313, 0.3333333333333333703, 0.3079598441704289313, 0.3333333333333333703, 0.3079598441704289313, 0.3333333333333333703, 0.3079598441704289313, 0.3333333333333333703, 0.3079598441704289313, 0.3333333333333333703, 0.3079598441704289313, 0.3333333333333333703, 0.3079598441704289313, 0.3333333333333333703, 0.3079598441704289313, 0.3333333333333333703, 0.3079598441704289313, 0.3333333333333333703, 0.3079598441704289313, 0.3333333333333333703, 0.3079598441704289313, 0.3333333333333333703, 0.3079598441704289313, 0.3333333333333333703, 0.3079598441704289313, 0.3333333333333333703, 0.3079598441704289313, 0.3333333333333333703, 0.3079598441704289313, 0.3333333333333333703, 0.3079598441704289313, 0.3333333333333333703, 0.3079598441704289313, 0.3333333333333333703, 0.3079598441704289313, 0.3333333333333333703, 0.3079598441704289313, 0.3333333333333333703, 0.3079598441704289313, 0.3333333333333333703, 0.3079598441704289313, 0.3333333333333333703, 0.3079598441704289313, 0.3333333333333333703, 0.3079598441704289313, 0.3333333333333333703, 0.3079598441704289313, 0.3333333333333333703, 0.3079598441704289313, 0.3333333333333333703, 0.3079598441704289313, 0.3333333333333333703, 0.3079598441704289313, 0.3333333333333333703, 0.3079598441704289313, 0.3333333333333333703, 0.3079598441704289313, 0.3333333333333333703, 0.3251605826665369681, 0.3222526856454325239),
 ( 1.000000000000000000, 0.9238795325112867385, 1.000000000000000000, 0.9238795325112867385, 1.000000000000000000, 0.9238795325112867385, 1.000000000000000000, 0.9238795325112867385, 1.000000000000000000, 0.9238795325112867385, 1.000000000000000000, 0.9238795325112867385, 1.000000000000000000, 0.9238795325112867385, 1.000000000000000000, 0.9238795325112867385, 1.000000000000000000, 0.9238795325112867385, 1.000000000000000000, 0.9238795325112867385, 1.000000000000000000, 0.9238795325112867385, 1.000000000000000000, 0.9238795325112867385, 1.000000000000000000, 0.9238795325112867385, 1.000000000000000000, 0.9238795325112867385, 1.000000000000000000, 0.9238795325112867385, 1.000000000000000000, 0.9238795325112867385, 1.000000000000000000, 0.9238795325112867385, 1.000000000000000000, 0.9238795325112867385, 1.000000000000000000, 0.9238795325112867385, 1.000000000000000000, 0.9238795325112867385, 1.000000000000000000, 0.9238795325112867385, 1.000000000000000000, 0.9238795325112867385, 1.000000000000000000, 0.9238795325112867385, 1.000000000000000000, 0.9238795325112867385, 1.000000000000000000, 0.9238795325112867385, 1.000000000000000000, 0.9238795325112867385, 1.000000000000000000, 0.9238795325112867385, 1.000000000000000000, 0.9238795325112867385, 1.000000000000000000, 0.9238795325112867385, 1.000000000000000000, 0.9238795325112867385, 1.000000000000000000, 0.9238795325112867385, 1.000000000000000000, 0.9238795325112867385, 1.000000000000000000, 0.9238795325112867385, 1.000000000000000000, 0.9238795325112867385, 1.000000000000000000, 0.9238795325112867385, 1.000000000000000000, 0.9238795325112867385, 1.000000000000000000, 0.9238795325112867385, 1.000000000000000000, 0.9238795325112867385, 1.000000000000000000, 0.9238795325112867385, 1.000000000000000000, 0.9238795325112867385, 1.000000000000000000, 0.9238795325112867385, 1.000000000000000000, 0.9238795325112867385, 1.000000000000000000, 0.9238795325112867385, 1.000000000000000000, 0.9238795325112867385, 1.000000000000000000, 0.9238795325112867385, 1.000000000000000000, 0.9238795325112867385, 1.000000000000000000, 0.9754817479996107377, 0.9667580569362973497) ) ) 
 REPRESENTATION_ITEM ( '' )  SURFACE ( )  );
#19800 = CARTESIAN_POINT ( 'NONE',  ( 19.19064177244175440, 10.00000000000000000, 1.000000000000000000 ) ) ;
#19801 = CARTESIAN_POINT ( 'NONE',  ( 0.9854920305337621089, -9.114917468222230923, 2.372643865078341019 ) ) ;
#19802 = VECTOR ( 'NONE', #2557, 1000.000000000000000 ) ;
#19803 = EDGE_CURVE ( 'NONE', #10907, #11591, #604, .T. ) ;
#19804 = CARTESIAN_POINT ( 'NONE',  ( 1.337453470010121714, -9.114917468222230923, 1.622643865078341463 ) ) ;
#19805 = CARTESIAN_POINT ( 'NONE',  ( -12.62499999998404299, -19.49999999996810729, 2.793053905886972998 ) ) ;
#19806 = CARTESIAN_POINT ( 'NONE',  ( 6.715308582316794173, -23.77099543870833998, 2.825813738724734847 ) ) ;
#19807 = DIRECTION ( 'NONE',  ( 1.000000000000000000, 0.000000000000000000, 0.000000000000000000 ) ) ;
#19808 = CARTESIAN_POINT ( 'NONE',  ( 12.62599079447150885, -20.19996487918709249, 4.820256282269618886 ) ) ;
#19809 = AXIS2_PLACEMENT_3D ( 'NONE', #5092, #19225, #16278 ) ;
#19810 = CARTESIAN_POINT ( 'NONE',  ( -2.817596665886821672, -11.50588678273290988, 2.986692549455723267 ) ) ;
#19811 = CARTESIAN_POINT ( 'NONE',  ( 8.309058582316795949, -22.74294823697954016, 2.828734674606448785 ) ) ;
#19812 = CARTESIAN_POINT ( 'NONE',  ( 6.815941417683176518, -20.79840458871654363, 4.773278322869464851 ) ) ;
#19813 = CARTESIAN_POINT ( 'NONE',  ( -10.84030858231679240, -22.67418626127525982, 5.270995438708342640 ) ) ;
#19814 = ORIENTED_EDGE ( 'NONE', *, *, #13573, .F. ) ;
#19815 = CARTESIAN_POINT ( 'NONE',  ( 13.13728495444130751, 4.870390199291127153, 6.548325014280736767 ) ) ;
#19816 = CARTESIAN_POINT ( 'NONE',  ( 12.62966097655984754, -19.26462068372267566, 4.756751955311774083 ) ) ;
#19817 = CARTESIAN_POINT ( 'NONE',  ( 17.12779268661489596, 11.64110105645932691, 10.00000000000000000 ) ) ;
#19818 = ORIENTED_EDGE ( 'NONE', *, *, #18283, .F. ) ;
#19819 = VERTEX_POINT ( 'NONE', #5520 ) ;
#19820 = CARTESIAN_POINT ( 'NONE',  ( 15.50000000000000178, -20.99999999999999645, 1.000000000000000000 ) ) ;
#19821 = VECTOR ( 'NONE', #18238, 1000.000000000000000 ) ;
#19822 = CARTESIAN_POINT ( 'NONE',  ( 10.18924542913430820, 0.000000000000000000, 1.000000000000000000 ) ) ;
#19823 = DIRECTION ( 'NONE',  ( 0.4999999999999947820, 0.8660254037844417052, -0.000000000000000000 ) ) ;
#19824 = DIRECTION ( 'NONE',  ( 0.000000000000000000, -1.000000000000000000, 0.000000000000000000 ) ) ;
#19825 = CARTESIAN_POINT ( 'NONE',  ( 1.716273078461125090, -9.866787073280026021, 2.373124017006284170 ) ) ;
#19826 = DIRECTION ( 'NONE',  ( 1.000000000000000000, 0.000000000000000000, 0.000000000000000000 ) ) ;
#19827 = DIRECTION ( 'NONE',  ( -0.000000000000000000, -0.000000000000000000, -1.000000000000000000 ) ) ;
#19828 = ADVANCED_FACE ( 'NONE', ( #913 ), #16811, .T. ) ;
#19829 = CARTESIAN_POINT ( 'NONE',  ( 12.87788743559736027, -20.60791989766740073, 3.516327362592114092 ) ) ;
#19830 = CARTESIAN_POINT ( 'NONE',  ( -1.824488249492779879, -9.124319963227819130, 2.375058613629473570 ) ) ;
#19831 = CARTESIAN_POINT ( 'NONE',  ( -8.496558582316794173, -22.05068747287764452, 1.749999999999998446 ) ) ;
#19832 = CARTESIAN_POINT ( 'NONE',  ( -3.506783328160878010, -9.991161114504492957, 2.040295720924476530 ) ) ;
#19833 = ORIENTED_EDGE ( 'NONE', *, *, #3640, .T. ) ;
#19834 = CARTESIAN_POINT ( 'NONE',  ( -13.37680511754115287, -19.40884156416817774, 4.692171866446762429 ) ) ;
#19835 = CARTESIAN_POINT ( 'NONE',  ( -5.590308582316794173, -21.32581373872472597, 1.729004561291657582 ) ) ;
#19836 = AXIS2_PLACEMENT_3D ( 'NONE', #17875, #6583, #14524 ) ;
#19837 = CARTESIAN_POINT ( 'NONE',  ( -4.003441417683176518, -22.05068747287765873, 5.250000000000000888 ) ) ;
#19838 = ORIENTED_EDGE ( 'NONE', *, *, #11605, .F. ) ;
#19839 = CARTESIAN_POINT ( 'NONE',  ( 13.37499999999998224, -20.24999999999998934, 4.166666666666636765 ) ) ;
#19840 = LINE ( 'NONE', #12078, #19084 ) ;
#19841 = ORIENTED_EDGE ( 'NONE', *, *, #9135, .T. ) ;
#19842 = ORIENTED_EDGE ( 'NONE', *, *, #12222, .F. ) ;
#19843 = CARTESIAN_POINT ( 'NONE',  ( 19.19064177244175440, 0.000000000000000000, 1.000000000000000000 ) ) ;
#19844 = ORIENTED_EDGE ( 'NONE', *, *, #12067, .F. ) ;
#19845 = CARTESIAN_POINT ( 'NONE',  ( -13.37883250981221472, -20.05645825448334563, 5.102688967256983510 ) ) ;
#19846 = VECTOR ( 'NONE', #5811, 1000.000000000000000 ) ;
#19847 = AXIS2_PLACEMENT_3D ( 'NONE', #3144, #6387, #1777 ) ;
#19848 = ORIENTED_EDGE ( 'NONE', *, *, #10520, .F. ) ;
#19849 = CARTESIAN_POINT ( 'NONE',  ( -21.42243175760212637, 9.000000000000001776, 1.000000000000000000 ) ) ;
#19850 = CARTESIAN_POINT ( 'NONE',  ( -9.805650798910056309, 9.000000000000001776, 1.000000000000000000 ) ) ;
#19851 = CARTESIAN_POINT ( 'NONE',  ( -17.11324865405191176, -11.00000000000000000, 2.000000000000000000 ) ) ;
#19852 = CARTESIAN_POINT ( 'NONE',  ( 3.379380450443691952, -10.24275229525297348, 2.854909362179569587 ) ) ;
#19853 = CARTESIAN_POINT ( 'NONE',  ( -4.687312169500630787, -21.51559725698340131, 5.182386163300424009 ) ) ;
#19854 = ADVANCED_FACE ( 'NONE', ( #8556 ), #19868, .F. ) ;
#19855 = CARTESIAN_POINT ( 'NONE',  ( 12.65679946139692902, -19.39412719945235253, 6.251687395662565372 ) ) ;
#19856 = CARTESIAN_POINT ( 'NONE',  ( -0.1250000000000001110, 10.00000000000000000, 1.000000000000000000 ) ) ;
#19857 = CARTESIAN_POINT ( 'NONE',  ( 9.534691417683177406, -20.97900456129164581, 3.136473910504570917 ) ) ;
#19858 = DIRECTION ( 'NONE',  ( -0.000000000000000000, -0.000000000000000000, -1.000000000000000000 ) ) ;
#19859 = CARTESIAN_POINT ( 'NONE',  ( -4.378441417683176518, -22.99999999999999645, 3.449312527122335048 ) ) ;
#19860 = CARTESIAN_POINT ( 'NONE',  ( -9.809058582316795949, -23.80360840875935935, 1.768074502826626260 ) ) ;
#19861 = ORIENTED_EDGE ( 'NONE', *, *, #10636, .F. ) ;
#19862 = EDGE_CURVE ( 'NONE', #12057, #16179, #18285, .T. ) ;
#19863 = CARTESIAN_POINT ( 'NONE',  ( 12.62499999999998401, -19.49999999999998934, 2.439580858552613751 ) ) ;
#19864 = CARTESIAN_POINT ( 'NONE',  ( -13.02818618459764188, 0.1109023222084986743, 5.923858176248589125 ) ) ;
#19865 = ORIENTED_EDGE ( 'NONE', *, *, #1709, .F. ) ;
#19866 = ADVANCED_FACE ( 'NONE', ( #16402 ), #15031, .F. ) ;
#19867 = CARTESIAN_POINT ( 'NONE',  ( -11.99999999999999645, -26.49999999999998934, 1.000000000000000000 ) ) ;
#19868 = PLANE ( 'NONE',  #8665 ) ;
#19869 = ORIENTED_EDGE ( 'NONE', *, *, #18347, .T. ) ;
#19870 = ORIENTED_EDGE ( 'NONE', *, *, #17797, .F. ) ;
#19871 = ORIENTED_EDGE ( 'NONE', *, *, #12470, .F. ) ;
#19872 = DIRECTION ( 'NONE',  ( 5.204170427930446527E-15, -1.000000000000000000, 0.000000000000000000 ) ) ;
#19873 = CARTESIAN_POINT ( 'NONE',  ( -13.81494360078803396, 11.64110105645932691, 0.000000000000000000 ) ) ;
#19874 = CARTESIAN_POINT ( 'NONE',  ( -1.548630333695928618, -8.364917468222230923, 1.622643865078341907 ) ) ;
#19875 = PLANE ( 'NONE',  #13694 ) ;
#19876 = DIRECTION ( 'NONE',  ( 1.000000000000000000, 0.000000000000000000, 0.000000000000000000 ) ) ;
#19877 = EDGE_CURVE ( 'NONE', #18643, #12338, #12108, .T. ) ;
#19878 = CARTESIAN_POINT ( 'NONE',  ( 13.12529380813666435, 5.014837310896125722, 5.033295791462342628 ) ) ;
#19879 = LINE ( 'NONE', #7423, #5684 ) ;
#19880 = CARTESIAN_POINT ( 'NONE',  ( 5.777808582316795949, -19.52099543870833642, 2.413778621189609286 ) ) ;
#19881 = CARTESIAN_POINT ( 'NONE',  ( -12.83635126708105823, -9.576761012430582198, 5.715524842913705328 ) ) ;
#19882 = CARTESIAN_POINT ( 'NONE',  ( -4.659691417683177406, -22.98484643305507191, 0.9790045612916508100 ) ) ;
#19883 = VERTEX_POINT ( 'NONE', #8461 ) ;
#19884 = CARTESIAN_POINT ( 'NONE',  ( -11.24178095869206828, 9.000000000000001776, 1.000000000000000000 ) ) ;
#19885 = LINE ( 'NONE', #4076, #7077 ) ;
#19886 = CARTESIAN_POINT ( 'NONE',  ( -13.56222317325195093, -11.54522975075300728, 6.408692769197242178 ) ) ;
#19887 = CARTESIAN_POINT ( 'NONE',  ( 4.840308582316795061, -22.36352608949544418, 4.520995438708343528 ) ) ;
#19888 = DIRECTION ( 'NONE',  ( 1.000000000000000000, 0.000000000000000000, -0.000000000000000000 ) ) ;
#19889 = ORIENTED_EDGE ( 'NONE', *, *, #8750, .F. ) ;
#19890 = ORIENTED_EDGE ( 'NONE', *, *, #4163, .F. ) ;
#19891 = CARTESIAN_POINT ( 'NONE',  ( 13.87454419214980739, 4.976981703567351367, 5.131312659523921127 ) ) ;
#19892 = VECTOR ( 'NONE', #16332, 1000.000000000000000 ) ;
#19893 = DIRECTION ( 'NONE',  ( -0.000000000000000000, 0.000000000000000000, -1.000000000000000000 ) ) ;
#19894 = VERTEX_POINT ( 'NONE', #19963 ) ;
#19895 = DIRECTION ( 'NONE',  ( 0.000000000000000000, 1.000000000000000000, -0.000000000000000000 ) ) ;
#19896 = DIRECTION ( 'NONE',  ( 0.000000000000000000, 1.000000000000000000, 0.000000000000000000 ) ) ;
#19897 = CARTESIAN_POINT ( 'NONE',  ( 10.05565079891005631, 9.000000000000001776, 1.000000000000000000 ) ) ;
#19898 = CARTESIAN_POINT ( 'NONE',  ( 13.39107665282975645, -19.43812903209671461, 5.476542851584349947 ) ) ;
#19899 = PLANE ( 'NONE',  #14187 ) ;
#19900 = CARTESIAN_POINT ( 'NONE',  ( 1.743623630681728542, -9.116095536440919744, 2.372946416531167557 ) ) ;
#19901 = EDGE_CURVE ( 'NONE', #20292, #740, #6990, .T. ) ;
#19902 = ADVANCED_FACE ( 'NONE', ( #2381 ), #13359, .T. ) ;
#19903 = LINE ( 'NONE', #10372, #7722 ) ;
#19904 = CARTESIAN_POINT ( 'NONE',  ( -13.12529397354238192, 5.014845663890295846, 4.583333333333296622 ) ) ;
#19905 = FACE_OUTER_BOUND ( 'NONE', #7555, .T. ) ;
#19906 = VECTOR ( 'NONE', #10707, 1000.000000000000000 ) ;
#19907 = CARTESIAN_POINT ( 'NONE',  ( 12.24655858231679240, -21.94931252712234482, 5.250000000000000888 ) ) ;
#19908 = CARTESIAN_POINT ( 'NONE',  ( -13.40787921250184311, -19.33959976865745389, 6.241060671539915283 ) ) ;
#19909 = EDGE_CURVE ( 'NONE', #19648, #19129, #14830, .T. ) ;
#19910 = DIRECTION ( 'NONE',  ( 0.000000000000000000, -0.000000000000000000, 1.000000000000000000 ) ) ;
#19911 = CARTESIAN_POINT ( 'NONE',  ( 11.40280858231679595, -22.46490103525074034, 2.520995438708341307 ) ) ;
#19912 = CARTESIAN_POINT ( 'NONE',  ( 10.28469141768318096, -23.77099543870834353, 4.174186261275252718 ) ) ;
#19913 = CARTESIAN_POINT ( 'NONE',  ( -11.49655858231679417, -22.05068747287764452, 1.749999999999998446 ) ) ;
#19914 = ORIENTED_EDGE ( 'NONE', *, *, #16608, .T. ) ;
#19915 = CARTESIAN_POINT ( 'NONE',  ( 13.11644927503132330, 3.818188389080370282, 6.753616037489316604 ) ) ;
#19916 = CARTESIAN_POINT ( 'NONE',  ( 12.62868952012632207, -19.31367923361656480, 4.748088538831167327 ) ) ;
#19917 = LINE ( 'NONE', #11942, #10683 ) ;
#19918 = EDGE_LOOP ( 'NONE', ( #9275, #10972, #20358, #6743 ) ) ;
#19919 = EDGE_CURVE ( 'NONE', #10855, #11555, #5309, .T. ) ;
#19920 = VERTEX_POINT ( 'NONE', #10226 ) ;
#19921 = PLANE ( 'NONE',  #12444 ) ;
#19922 = FACE_OUTER_BOUND ( 'NONE', #2225, .T. ) ;
#19923 = CARTESIAN_POINT ( 'NONE',  ( 20.50349085826861995, 10.00000000000000000, 1.000000000000000000 ) ) ;
#19924 = CARTESIAN_POINT ( 'NONE',  ( 30.00000000000000000, 0.000000000000000000, 0.000000000000000000 ) ) ;
#19925 = CARTESIAN_POINT ( 'NONE',  ( 1.619022621591187150, -9.114917468222230923, 2.372643865078341019 ) ) ;
#19926 = CARTESIAN_POINT ( 'NONE',  ( 13.00209451496117374, 11.64110105645932691, 10.00000000000000000 ) ) ;
#19927 = CARTESIAN_POINT ( 'NONE',  ( 18.44064177244175440, 0.000000000000000000, 1.000000000000000000 ) ) ;
#19928 = CARTESIAN_POINT ( 'NONE',  ( 0.000000000000000000, 9.000000000000001776, 0.000000000000000000 ) ) ;
#19929 = CARTESIAN_POINT ( 'NONE',  ( -2.601332995093193379, -9.970398767539743190, 2.592349323443654097 ) ) ;
#19930 = CARTESIAN_POINT ( 'NONE',  ( -5.871558582316794173, -20.24999999999999289, 3.449312527122348371 ) ) ;
#19931 = CARTESIAN_POINT ( 'NONE',  ( -3.436477319925839602, -9.631595465688135960, 1.947952079262935676 ) ) ;
#19932 = EDGE_LOOP ( 'NONE', ( #4056, #4347, #4744, #15732 ) ) ;
#19933 = CARTESIAN_POINT ( 'NONE',  ( -13.37893135632597819, -19.30146650553847465, 4.738802066438188909 ) ) ;
#19934 = CARTESIAN_POINT ( 'NONE',  ( 4.000698171653723101, 10.00000000000000000, 1.000000000000000000 ) ) ;
#19935 = CARTESIAN_POINT ( 'NONE',  ( 12.15280858231679950, -20.91377862118960351, 5.979004561291660913 ) ) ;
#19936 = CARTESIAN_POINT ( 'NONE',  ( -11.31594141768317741, -21.32873467460645145, 4.242948236979555254 ) ) ;
#19937 = ORIENTED_EDGE ( 'NONE', *, *, #3993, .T. ) ;
#19938 = CARTESIAN_POINT ( 'NONE',  ( 13.84264281492353987, 3.365962153638767607, 5.979325532956542233 ) ) ;
#19939 = CARTESIAN_POINT ( 'NONE',  ( -2.693754455098655409, -10.04853567022903782, 2.237415670251142519 ) ) ;
#19940 = VERTEX_POINT ( 'NONE', #7300 ) ;
#19941 = ORIENTED_EDGE ( 'NONE', *, *, #13480, .F. ) ;
#19942 = ADVANCED_FACE ( 'NONE', ( #19761 ), #2271, .F. ) ;
#19943 = DIRECTION ( 'NONE',  ( -0.000000000000000000, -0.000000000000000000, -1.000000000000000000 ) ) ;
#19944 = ORIENTED_EDGE ( 'NONE', *, *, #5995, .F. ) ;
#19945 = CARTESIAN_POINT ( 'NONE',  ( -13.37500015856764435, -20.24999199233421265, 4.532157119432948633 ) ) ;
#19946 = ORIENTED_EDGE ( 'NONE', *, *, #13605, .T. ) ;
#19947 = DIRECTION ( 'NONE',  ( -0.000000000000000000, 0.000000000000000000, -1.000000000000000000 ) ) ;
#19948 = CARTESIAN_POINT ( 'NONE',  ( -18.98630159782011262, 0.000000000000000000, 0.000000000000000000 ) ) ;
#19949 = CARTESIAN_POINT ( 'NONE',  ( 0.000000000000000000, 0.000000000000000000, 1.000000000000000000 ) ) ;
#19950 = CARTESIAN_POINT ( 'NONE',  ( 3.451187703687236041, -10.75258211228477734, 2.985843844067104680 ) ) ;
#19951 = CARTESIAN_POINT ( 'NONE',  ( -6.434058582316794173, -23.20159541128345992, 4.773278322869455970 ) ) ;
#19952 = CARTESIAN_POINT ( 'NONE',  ( 13.87486364728600208, 4.243114187942282456, 6.725269602253773016 ) ) ;
#19953 = CARTESIAN_POINT ( 'NONE',  ( 0.000000000000000000, 9.000000000000001776, 1.000000000000000000 ) ) ;
#19954 = CARTESIAN_POINT ( 'NONE',  ( 4.190941417683176518, -23.27327832286946219, 4.701595411283453707 ) ) ;
#19955 = DIRECTION ( 'NONE',  ( 1.000000000000000000, 0.000000000000000000, 0.000000000000000000 ) ) ;
#19956 = CARTESIAN_POINT ( 'NONE',  ( -4.190941417683176518, -22.74294823697955081, 4.171265325393542334 ) ) ;
#19957 = CARTESIAN_POINT ( 'NONE',  ( -10.56594141768317741, -23.73192549717336064, 1.696391591240623331 ) ) ;
#19958 = VERTEX_POINT ( 'NONE', #503 ) ;
#19959 = CARTESIAN_POINT ( 'NONE',  ( 12.64917329730235096, -18.27924848622803466, 4.778345106674467324 ) ) ;
#19960 = CARTESIAN_POINT ( 'NONE',  ( -13.11145189917479392, 4.315820908324673688, 5.961432613039677086 ) ) ;
#19961 = EDGE_LOOP ( 'NONE', ( #8560, #5310, #20462, #6291 ) ) ;
#19962 = CARTESIAN_POINT ( 'NONE',  ( 0.000000000000000000, 9.000000000000001776, 1.000000000000000000 ) ) ;
#19963 = CARTESIAN_POINT ( 'NONE',  ( 14.50000000000001243, -25.49999999999999645, 1.000000000000000000 ) ) ;
#19964 = VERTEX_POINT ( 'NONE', #5625 ) ;
#19965 = ITEM_DEFINED_TRANSFORMATION ( 'NONE', 'NONE', #18,  #18039 ) ;
#19966 = VECTOR ( 'NONE', #12636, 1000.000000000000000 ) ;
#19967 = EDGE_LOOP ( 'NONE', ( #14930, #1820, #6357, #12004 ) ) ;
#19968 = EDGE_CURVE ( 'NONE', #11652, #17187, #9990, .T. ) ;
#19969 = VERTEX_POINT ( 'NONE', #10128 ) ;
#19970 = DIRECTION ( 'NONE',  ( 0.000000000000000000, 1.000000000000000000, 0.000000000000000000 ) ) ;
#19971 = CARTESIAN_POINT ( 'NONE',  ( 10.18924542913430820, 10.00000000000000000, 1.000000000000000000 ) ) ;
#19972 = CARTESIAN_POINT ( 'NONE',  ( -1.619022621591187150, -9.114917468222230923, 1.622643865078341463 ) ) ;
#19973 = CARTESIAN_POINT ( 'NONE',  ( -4.000000000000000000, -8.500000000000000000, 1.000000000000000000 ) ) ;
#19974 = FACE_OUTER_BOUND ( 'NONE', #17801, .T. ) ;
#19975 = EDGE_CURVE ( 'NONE', #11061, #2483, #15241, .T. ) ;
#19976 = CARTESIAN_POINT ( 'NONE',  ( 13.00209451496117374, 10.00000000000000000, 1.000000000000000000 ) ) ;
#19977 = CARTESIAN_POINT ( 'NONE',  ( 6.621558582316796837, -24.50000000000000000, 3.550687472877651629 ) ) ;
#19978 = CARTESIAN_POINT ( 'NONE',  ( -13.10252221513633941, 3.864871864382954048, 6.004587342915129966 ) ) ;
#19979 = CARTESIAN_POINT ( 'NONE',  ( -6.815941417683177406, -20.26807450282663225, 5.303608408759377113 ) ) ;
#19980 = EDGE_LOOP ( 'NONE', ( #2427, #9465, #20492, #271 ) ) ;
#19981 = CARTESIAN_POINT ( 'NONE',  ( 11.87155858231679417, -20.24999999999999289, 3.449312527122348371 ) ) ;
#19982 = CYLINDRICAL_SURFACE ( 'NONE', #12085, 1.000000000000002665 ) ;
#19983 = CARTESIAN_POINT ( 'NONE',  ( -13.42074492158312715, -18.68988146005270679, 6.255046935864005064 ) ) ;
#19984 = CARTESIAN_POINT ( 'NONE',  ( 12.34030858231679240, -22.67418626127525982, 5.270995438708342640 ) ) ;
#19985 = DIRECTION ( 'NONE',  ( -1.000000000000000000, 0.000000000000000000, 0.000000000000000000 ) ) ;
#19986 = ORIENTED_EDGE ( 'NONE', *, *, #15869, .T. ) ;
#19987 = ORIENTED_EDGE ( 'NONE', *, *, #664, .F. ) ;
#19988 = CARTESIAN_POINT ( 'NONE',  ( 13.47096266223369376, -15.40388555723029462, 5.575679699623145247 ) ) ;
#19989 = CARTESIAN_POINT ( 'NONE',  ( 0.000000000000000000, 4.999999999999999112, 1.000000000000000000 ) ) ;
#19990 = VERTEX_POINT ( 'NONE', #16500 ) ;
#19991 = ADVANCED_FACE ( 'NONE', ( #6883 ), #2173, .T. ) ;
#19992 = VECTOR ( 'NONE', #3320, 1000.000000000000000 ) ;
#19993 = CARTESIAN_POINT ( 'NONE',  ( 15.86404127825609400, 9.000000000000001776, 0.000000000000000000 ) ) ;
#19994 = DIRECTION ( 'NONE',  ( -0.000000000000000000, -0.000000000000000000, -1.000000000000000000 ) ) ;
#19995 = VECTOR ( 'NONE', #8020, 1000.000000000000000 ) ;
#19996 = DIRECTION ( 'NONE',  ( 1.000000000000000000, -0.000000000000000000, 0.000000000000000000 ) ) ;
#19997 = FACE_OUTER_BOUND ( 'NONE', #5627, .T. ) ;
#19998 = PLANE ( 'NONE',  #15194 ) ;
#19999 = CARTESIAN_POINT ( 'NONE',  ( 3.422464802389687311, -10.54865018547243061, 2.933470051312085936 ) ) ;
#20000 = LINE ( 'NONE', #5972, #1375 ) ;
#20001 = CARTESIAN_POINT ( 'NONE',  ( -13.12529418130016445, 5.014856155665242454, 4.958178834604180629 ) ) ;
#20002 = LINE ( 'NONE', #14191, #6963 ) ;
#20003 = VECTOR ( 'NONE', #13670, 1000.000000000000000 ) ;
#20004 = PLANE ( 'NONE',  #10072 ) ;
#20005 = CARTESIAN_POINT ( 'NONE',  ( -13.82120031190154208, 1.533115751011936867, 6.689942769197355865 ) ) ;
#20006 = ADVANCED_FACE ( 'NONE', ( #14360 ), #15731, .T. ) ;
#20007 = VECTOR ( 'NONE', #10059, 1000.000000000000000 ) ;
#20008 = LINE ( 'NONE', #5671, #3694 ) ;
#20009 = CARTESIAN_POINT ( 'NONE',  ( 5.309058582316795949, -22.74294823697954016, 2.828734674606448785 ) ) ;
#20010 = CARTESIAN_POINT ( 'NONE',  ( 4.659691417683178294, -22.67418626127524917, 1.729004561291651809 ) ) ;
#20011 = CARTESIAN_POINT ( 'NONE',  ( -10.27780858231679417, -20.27099543870833642, 2.724438792969431589 ) ) ;
#20012 = ORIENTED_EDGE ( 'NONE', *, *, #1937, .T. ) ;
#20013 = CARTESIAN_POINT ( 'NONE',  ( 13.11704875914858270, 3.848462337001107070, 6.754267079155989784 ) ) ;
#20014 = CARTESIAN_POINT ( 'NONE',  ( 13.07840392524817474, 3.396898225032857432, 5.244490940007585422 ) ) ;
#20015 = CARTESIAN_POINT ( 'NONE',  ( -0.1250000000000035805, 9.000000000000000000, 1.000000000000000000 ) ) ;
#20016 = ORIENTED_EDGE ( 'NONE', *, *, #11829, .F. ) ;
#20017 = EDGE_CURVE ( 'NONE', #16495, #7639, #18985, .T. ) ;
#20018 = VERTEX_POINT ( 'NONE', #15831 ) ;
#20019 = ADVANCED_FACE ( 'NONE', ( #20563 ), #1607, .T. ) ;
#20020 = LINE ( 'NONE', #5683, #12779 ) ;
#20021 = VECTOR ( 'NONE', #15632, 1000.000000000000000 ) ;
#20022 = AXIS2_PLACEMENT_3D ( 'NONE', #10109, #16485, #6564 ) ;
#20023 = LINE ( 'NONE', #8722, #6577 ) ;
#20024 = AXIS2_PLACEMENT_3D ( 'NONE', #20407, #13795, #5860 ) ;
#20025 = LINE ( 'NONE', #10497, #6648 ) ;
#20026 = CARTESIAN_POINT ( 'NONE',  ( 8.126396343307449754, 0.000000000000000000, 0.000000000000000000 ) ) ;
#20027 = CARTESIAN_POINT ( 'NONE',  ( 1.791727654783324741, -9.894249715907907472, 2.380176972254574697 ) ) ;
#20028 = DIRECTION ( 'NONE',  ( 0.000000000000000000, -0.000000000000000000, 1.000000000000000000 ) ) ;
#20029 = CARTESIAN_POINT ( 'NONE',  ( 0.000000000000000000, 16.00000000000000000, 1.000000000000000000 ) ) ;
#20030 = EDGE_CURVE ( 'NONE', #8332, #17247, #4641, .T. ) ;
#20031 = DIRECTION ( 'NONE',  ( 0.000000000000000000, -1.000000000000000000, 0.000000000000000000 ) ) ;
#20032 = CARTESIAN_POINT ( 'NONE',  ( -9.621558582316795949, -24.50000000000000000, 3.550687472877651629 ) ) ;
#20033 = CARTESIAN_POINT ( 'NONE',  ( -2.012076196476103362, -9.160103213191565175, 1.634248467062433541 ) ) ;
#20034 = VECTOR ( 'NONE', #18683, 1000.000000000000000 ) ;
#20035 = VERTEX_POINT ( 'NONE', #12206 ) ;
#20036 = CARTESIAN_POINT ( 'NONE',  ( -13.09560260347216953, 4.265431475339161338, 5.020858537328734883 ) ) ;
#20037 = CARTESIAN_POINT ( 'NONE',  ( -8.309058582316792396, -23.27327832286945153, 2.298404588716537411 ) ) ;
#20038 = CARTESIAN_POINT ( 'NONE',  ( 9.440941417683177406, -20.19639159124061933, 1.768074502826635586 ) ) ;
#20039 = CARTESIAN_POINT ( 'NONE',  ( -8.597191417683177406, -22.46490103525075810, 4.479004561291653808 ) ) ;
#20040 = CIRCLE ( 'NONE', #14677, 10.00000000000000000 ) ;
#20041 = ORIENTED_EDGE ( 'NONE', *, *, #11501, .T. ) ;
#20042 = CARTESIAN_POINT ( 'NONE',  ( 13.85343352903393388, 3.910893216212274925, 5.991044282956552891 ) ) ;
#20043 = CARTESIAN_POINT ( 'NONE',  ( -14.99999999999999645, -30.00000000000000711, 1.000000000000000000 ) ) ;
#20044 = ORIENTED_EDGE ( 'NONE', *, *, #471, .F. ) ;
#20045 = VERTEX_POINT ( 'NONE', #6317 ) ;
#20046 = DIRECTION ( 'NONE',  ( 1.000000000000000000, 0.000000000000000000, 0.000000000000000000 ) ) ;
#20047 = ORIENTED_EDGE ( 'NONE', *, *, #11235, .F. ) ;
#20048 = EDGE_CURVE ( 'NONE', #6320, #3666, #2584, .T. ) ;
#20049 = CARTESIAN_POINT ( 'NONE',  ( -13.80667376788930056, 1.549525278393783179, 5.940263032956496048 ) ) ;
#20050 = AXIS2_PLACEMENT_3D ( 'NONE', #6517, #16510, #16026 ) ;
#20051 = VERTEX_POINT ( 'NONE', #16046 ) ;
#20052 = FACE_OUTER_BOUND ( 'NONE', #6715, .T. ) ;
#20053 = CARTESIAN_POINT ( 'NONE',  ( 0.000000000000000000, 9.000000000000001776, 0.000000000000000000 ) ) ;
#20054 = STYLED_ITEM ( 'NONE', ( #3874 ), #17535 ) ;
#20055 = CARTESIAN_POINT ( 'NONE',  ( -17.05017143803810242, 4.999999999999999112, 0.000000000000000000 ) ) ;
#20056 = CARTESIAN_POINT ( 'NONE',  ( 3.270401025279431995, -9.547343748290430199, 2.676314555138040063 ) ) ;
#20057 = CARTESIAN_POINT ( 'NONE',  ( 2.693754455098655409, -10.14181605509423711, 1.874202551270839123 ) ) ;
#20058 = ADVANCED_FACE ( 'NONE', ( #8968 ), #7413, .T. ) ;
#20059 = VECTOR ( 'NONE', #16214, 1000.000000000000000 ) ;
#20060 = CARTESIAN_POINT ( 'NONE',  ( 12.66144083004408571, -19.15973808277258073, 6.259475412489329038 ) ) ;
#20061 = LINE ( 'NONE', #11577, #10634 ) ;
#20062 = PLANE ( 'NONE',  #18062 ) ;
#20063 = CARTESIAN_POINT ( 'NONE',  ( 4.097191417683176518, -22.77556120703057729, 5.229004561291655584 ) ) ;
#20064 = LINE ( 'NONE', #12198, #4866 ) ;
#20065 = CARTESIAN_POINT ( 'NONE',  ( -8.690941417683177406, -22.74294823697955081, 4.171265325393542334 ) ) ;
#20066 = CARTESIAN_POINT ( 'NONE',  ( -11.69094141768317741, -23.80360840875937001, 5.231925497173365081 ) ) ;
#20067 = VERTEX_POINT ( 'NONE', #11231 ) ;
#20068 = CARTESIAN_POINT ( 'NONE',  ( 13.12529397354238192, 5.014845663890295846, 4.333333333333382775 ) ) ;
#20069 = CARTESIAN_POINT ( 'NONE',  ( -12.64751377014909828, -19.11305460747000495, 5.510446717915143289 ) ) ;
#20070 = ORIENTED_EDGE ( 'NONE', *, *, #1913, .F. ) ;
#20071 = CARTESIAN_POINT ( 'NONE',  ( -26.19203811574920593, 10.00000000000000000, 1.000000000000000000 ) ) ;
#20072 = DIRECTION ( 'NONE',  ( -0.000000000000000000, -0.000000000000000000, -1.000000000000000000 ) ) ;
#20073 = ORIENTED_EDGE ( 'NONE', *, *, #20048, .F. ) ;
#20074 = ORIENTED_EDGE ( 'NONE', *, *, #15603, .T. ) ;
#20075 = VECTOR ( 'NONE', #7597, 1000.000000000000000 ) ;
#20076 = ORIENTED_EDGE ( 'NONE', *, *, #19370, .F. ) ;
#20077 = CARTESIAN_POINT ( 'NONE',  ( -9.000000000000000000, -9.999999999999992895, 2.000000000000000000 ) ) ;
#20078 = CARTESIAN_POINT ( 'NONE',  ( 0.000000000000000000, 0.000000000000000000, 1.000000000000000000 ) ) ;
#20079 = CARTESIAN_POINT ( 'NONE',  ( -1.548630333695928396, -9.114917468222230923, 1.622643865078341463 ) ) ;
#20080 = CARTESIAN_POINT ( 'NONE',  ( -11.00000000000000000, -24.49999999999999289, 5.000000000000000000 ) ) ;
#20081 = LINE ( 'NONE', #17336, #362 ) ;
#20082 = LINE ( 'NONE', #7314, #7014 ) ;
#20083 = CARTESIAN_POINT ( 'NONE',  ( 5.496558582316795949, -22.05068747287764452, 0.9999999999999978906 ) ) ;
#20084 = CARTESIAN_POINT ( 'NONE',  ( -12.68288333306630378, -17.32689168014509207, 5.548858176248425700 ) ) ;
#20085 = VECTOR ( 'NONE', #18566, 1000.000000000000000 ) ;
#20086 = CARTESIAN_POINT ( 'NONE',  ( -8.034691417683175629, -19.47900456129164581, 2.515153566944927199 ) ) ;
#20087 = VECTOR ( 'NONE', #9453, 1000.000000000000000 ) ;
#20088 = EDGE_CURVE ( 'NONE', #17295, #5898, #13774, .T. ) ;
#20089 = AXIS2_PLACEMENT_3D ( 'NONE', #20310, #7342, #15177 ) ;
#20090 = VERTEX_POINT ( 'NONE', #1508 ) ;
#20091 = DIRECTION ( 'NONE',  ( 0.000000000000000000, 1.000000000000000000, 0.000000000000000000 ) ) ;
#20092 = DIRECTION ( 'NONE',  ( 1.000000000000000000, 0.000000000000000000, 0.000000000000000000 ) ) ;
#20093 = CARTESIAN_POINT ( 'NONE',  ( -13.37499999999998224, -20.99999999999991829, 4.333333333333343695 ) ) ;
#20094 = CARTESIAN_POINT ( 'NONE',  ( 5.309058582316795949, -22.74294823697954016, 2.828734674606448785 ) ) ;
#20095 = CARTESIAN_POINT ( 'NONE',  ( -26.94203811574920593, 10.00000000000000000, 1.000000000000000000 ) ) ;
#20096 = VERTEX_POINT ( 'NONE', #3183 ) ;
#20097 = ORIENTED_EDGE ( 'NONE', *, *, #2132, .F. ) ;
#20098 = CARTESIAN_POINT ( 'NONE',  ( 13.37499999999998224, -20.99999999999998934, 4.166666666666637653 ) ) ;
#20099 = PLANE ( 'NONE',  #1879 ) ;
#20100 = SHAPE_REPRESENTATION_RELATIONSHIP ( 'NONE' , 'NONE' ,  #14706, #17535 ) ;
#20101 = VERTEX_POINT ( 'NONE', #16911 ) ;
#20102 = DIRECTION ( 'NONE',  ( -0.000000000000000000, -0.000000000000000000, -1.000000000000000000 ) ) ;
#20103 = FACE_OUTER_BOUND ( 'NONE', #14351, .T. ) ;
#20104 = CARTESIAN_POINT ( 'NONE',  ( -10.74655858231679417, -21.94931252712234482, 5.250000000000000888 ) ) ;
#20105 = VECTOR ( 'NONE', #470, 1000.000000000000000 ) ;
#20106 = DIRECTION ( 'NONE',  ( 0.000000000000000000, 1.000000000000000000, 0.000000000000000000 ) ) ;
#20107 = DIRECTION ( 'NONE',  ( -0.000000000000000000, 0.000000000000000000, -1.000000000000000000 ) ) ;
#20108 = CARTESIAN_POINT ( 'NONE',  ( 1.407845757905374695, -8.364917468222230923, 1.622643865078341907 ) ) ;
#20109 = CARTESIAN_POINT ( 'NONE',  ( 0.000000000000000000, 4.999999999999999112, 0.000000000000000000 ) ) ;
#20110 = CARTESIAN_POINT ( 'NONE',  ( -13.09543520949579865, 4.256978079540234106, 5.067654010725516578 ) ) ;
#20111 = DIRECTION ( 'NONE',  ( 1.000000000000000000, 0.000000000000000000, 0.000000000000000000 ) ) ;
#20112 = CARTESIAN_POINT ( 'NONE',  ( -13.37923893525309715, -20.78593376972237650, 5.366589449429977954 ) ) ;
#20113 = ADVANCED_FACE ( 'NONE', ( #18597 ), #17608, .T. ) ;
#20114 = DIRECTION ( 'NONE',  ( 0.000000000000000000, -0.000000000000000000, -1.000000000000000000 ) ) ;
#20115 = CARTESIAN_POINT ( 'NONE',  ( 5.121558582316795061, -22.99999999999999645, 3.550687472877652073 ) ) ;
#20116 = VECTOR ( 'NONE', #11708, 1000.000000000000000 ) ;
#20117 = CARTESIAN_POINT ( 'NONE',  ( 5.315941417683176518, -20.79840458871654363, 4.773278322869464851 ) ) ;
#20118 = CARTESIAN_POINT ( 'NONE',  ( -9.152808582316794173, -21.22443879296942626, 5.229004561291659137 ) ) ;
#20119 = VERTEX_POINT ( 'NONE', #20177 ) ;
#20120 = ADVANCED_FACE ( 'NONE', ( #1024 ), #6431, .T. ) ;
#20121 = CARTESIAN_POINT ( 'NONE',  ( 13.08919463935856697, 3.941829287606363863, 5.256209690007596080 ) ) ;
#20122 = ADVANCED_FACE ( 'NONE', ( #10643 ), #14249, .T. ) ;
#20123 = DIRECTION ( 'NONE',  ( 0.000000000000000000, -0.000000000000000000, 1.000000000000000000 ) ) ;
#20124 = ORIENTED_EDGE ( 'NONE', *, *, #155, .F. ) ;
#20125 = UNCERTAINTY_MEASURE_WITH_UNIT (LENGTH_MEASURE( 1.000000000000000082E-05 ), #6364, 'distance_accuracy_value', 'NONE');
#20126 = ORIENTED_EDGE ( 'NONE', *, *, #2061, .F. ) ;
#20127 = CARTESIAN_POINT ( 'NONE',  ( 0.000000000000000000, 16.00000000000000000, 1.000000000000000000 ) ) ;
#20128 = CARTESIAN_POINT ( 'NONE',  ( -5.381197846483055436, -6.000000000000000000, 2.000000000000000000 ) ) ;
#20129 = CARTESIAN_POINT ( 'NONE',  ( -2.702705060698113115, -10.69015907548275379, 2.777197378435510622 ) ) ;
#20130 = CARTESIAN_POINT ( 'NONE',  ( -13.43259567872942917, -17.34141822415733714, 5.534013032956523581 ) ) ;
#20131 = VECTOR ( 'NONE', #8233, 1000.000000000000000 ) ;
#20132 = DIRECTION ( 'NONE',  ( -0.1736481776669293042, 0.9848077530122082424, 0.000000000000000000 ) ) ;
#20133 = CARTESIAN_POINT ( 'NONE',  ( 1.837882866761050282, -9.938290523052360825, 2.391487531332776140 ) ) ;
#20134 = LINE ( 'NONE', #15199, #17167 ) ;
#20135 = DIRECTION ( 'NONE',  ( -0.000000000000000000, -0.000000000000000000, -1.000000000000000000 ) ) ;
#20136 = EDGE_CURVE ( 'NONE', #8942, #13028, #9011, .T. ) ;
#20137 = CARTESIAN_POINT ( 'NONE',  ( 0.000000000000000000, 9.000000000000001776, 1.000000000000000000 ) ) ;
#20138 = CARTESIAN_POINT ( 'NONE',  ( -12.99655858231679595, -22.05068747287764452, 0.9999999999999978906 ) ) ;
#20139 = CARTESIAN_POINT ( 'NONE',  ( -2.768424032093183662, -10.00067216410020166, 1.850123365707658785 ) ) ;
#20140 = EDGE_LOOP ( 'NONE', ( #19838, #19448, #17599, #18991 ) ) ;
#20141 = CARTESIAN_POINT ( 'NONE',  ( -13.37818000216760694, -19.33940989053615311, 4.728953261990445966 ) ) ;
#20142 = CARTESIAN_POINT ( 'NONE',  ( 13.50000000000001243, -24.49999999999999289, 4.000000000000000000 ) ) ;
#20143 = CARTESIAN_POINT ( 'NONE',  ( 5.027808582316795949, -24.47900456129166358, 4.586221378810390270 ) ) ;
#20144 = CARTESIAN_POINT ( 'NONE',  ( -12.44094141768317741, -21.25705176302044208, 2.828734674606458555 ) ) ;
#20145 = ORIENTED_EDGE ( 'NONE', *, *, #11498, .T. ) ;
#20146 = CARTESIAN_POINT ( 'NONE',  ( 13.37515323800563039, -20.24226148071262799, 4.627790572011877934 ) ) ;
#20147 = DIRECTION ( 'NONE',  ( 2.312964634635730039E-15, -1.000000000000000000, 0.000000000000000000 ) ) ;
#20148 = VERTEX_POINT ( 'NONE', #2694 ) ;
#20149 = ORIENTED_EDGE ( 'NONE', *, *, #12484, .F. ) ;
#20150 = VECTOR ( 'NONE', #11823, 1000.000000000000000 ) ;
#20151 = CARTESIAN_POINT ( 'NONE',  ( 12.25209451496117197, 0.000000000000000000, 1.000000000000000000 ) ) ;
#20152 = ORIENTED_EDGE ( 'NONE', *, *, #1736, .F. ) ;
#20153 = CARTESIAN_POINT ( 'NONE',  ( -13.84863765609603625, 3.668701632846259830, 5.985835949623216301 ) ) ;
#20154 = CARTESIAN_POINT ( 'NONE',  ( 1.904508877737772998, -9.138371295333994837, 2.378667276417936627 ) ) ;
#20155 = VERTEX_POINT ( 'NONE', #12691 ) ;
#20156 = LINE ( 'NONE', #5817, #11524 ) ;
#20157 = DIRECTION ( 'NONE',  ( 0.000000000000000000, 0.000000000000000000, -1.000000000000000000 ) ) ;
#20158 = CARTESIAN_POINT ( 'NONE',  ( -0.000000000000000000, 11.64110105645932691, 0.000000000000000000 ) ) ;
#20159 = CARTESIAN_POINT ( 'NONE',  ( 3.365018999794965548, -10.14078633184679923, 2.828722465802024910 ) ) ;
#20160 = FACE_OUTER_BOUND ( 'NONE', #5117, .T. ) ;
#20161 = AXIS2_PLACEMENT_3D ( 'NONE', #18000, #17899, #16232 ) ;
#20162 = EDGE_CURVE ( 'NONE', #6206, #2900, #12795, .T. ) ;
#20163 = CARTESIAN_POINT ( 'NONE',  ( 12.66383876651304874, -19.03864229108970463, 6.262079579155994224 ) ) ;
#20164 = DIRECTION ( 'NONE',  ( 0.000000000000000000, -0.9659258262890672020, 0.2588190451025246253 ) ) ;
#20165 = CARTESIAN_POINT ( 'NONE',  ( 0.6250000000000005551, 0.000000000000000000, 1.000000000000000000 ) ) ;
#20166 = ADVANCED_FACE ( 'NONE', ( #7989 ), #19197, .T. ) ;
#20167 = CARTESIAN_POINT ( 'NONE',  ( -5.563547257480587760, 11.64110105645932691, 0.000000000000000000 ) ) ;
#20168 = CARTESIAN_POINT ( 'NONE',  ( 3.974842109207561425, -21.82955800590261575, 5.256404853634145447 ) ) ;
#20169 = FACE_OUTER_BOUND ( 'NONE', #7274, .T. ) ;
#20170 = CARTESIAN_POINT ( 'NONE',  ( -9.527808582316795949, -22.97900456129165647, 3.964901035250747885 ) ) ;
#20171 = CARTESIAN_POINT ( 'NONE',  ( -8.878441417683177406, -24.50000000000000000, 3.449312527122335048 ) ) ;
#20172 = ORIENTED_EDGE ( 'NONE', *, *, #13616, .T. ) ;
#20173 = CARTESIAN_POINT ( 'NONE',  ( 12.62499999999998401, -19.49999999999998934, 3.146526952850934755 ) ) ;
#20174 = CARTESIAN_POINT ( 'NONE',  ( -13.12529397354238192, 5.014845663890295846, 4.833333333333344584 ) ) ;
#20175 = VERTEX_POINT ( 'NONE', #6632 ) ;
#20176 = CARTESIAN_POINT ( 'NONE',  ( 5.683390479346035029, 4.999999999999999112, 0.000000000000000000 ) ) ;
#20177 = CARTESIAN_POINT ( 'NONE',  ( 18.44064177244175440, 11.64110105645932691, 0.000000000000000000 ) ) ;
#20178 = VECTOR ( 'NONE', #19465, 1000.000000000000000 ) ;
#20179 = ORIENTED_EDGE ( 'NONE', *, *, #10396, .T. ) ;
#20180 = CARTESIAN_POINT ( 'NONE',  ( 1.857501949683560971, -9.975525523312803955, 2.401050223243493154 ) ) ;
#20181 = ORIENTED_EDGE ( 'NONE', *, *, #9898, .F. ) ;
#20182 = EDGE_CURVE ( 'NONE', #9838, #7608, #19509, .T. ) ;
#20183 = APPLICATION_CONTEXT ( 'automotive_design' ) ;
#20184 = ORIENTED_EDGE ( 'NONE', *, *, #13519, .T. ) ;
#20185 = CARTESIAN_POINT ( 'NONE',  ( -0.1250000000000001110, 0.000000000000000000, 1.000000000000000000 ) ) ;
#20186 = DIRECTION ( 'NONE',  ( 0.000000000000000000, 1.000000000000000000, -0.000000000000000000 ) ) ;
#20187 = CARTESIAN_POINT ( 'NONE',  ( 0.000000000000000000, -9.864917468222230923, 1.622643865078341241 ) ) ;
#20188 = CARTESIAN_POINT ( 'NONE',  ( 15.00000000000000355, -30.00000000000000000, 1.000000000000000000 ) ) ;
#20189 = DIRECTION ( 'NONE',  ( 0.1351665943404306014, -0.9596796555888912339, 0.2464649070825229438 ) ) ;
#20190 = DIRECTION ( 'NONE',  ( -0.000000000000000000, -0.000000000000000000, -1.000000000000000000 ) ) ;
#20191 = CARTESIAN_POINT ( 'NONE',  ( 9.815941417683177406, -20.26807450282663225, 5.303608408759377113 ) ) ;
#20192 = CARTESIAN_POINT ( 'NONE',  ( -12.65410809543883985, -18.78004118034163739, 5.517608176248461227 ) ) ;
#20193 = CARTESIAN_POINT ( 'NONE',  ( -6.159691417683175629, -22.98484643305507191, 0.9790045612916508100 ) ) ;
#20194 = ORIENTED_EDGE ( 'NONE', *, *, #17412, .T. ) ;
#20195 = CARTESIAN_POINT ( 'NONE',  ( -11.00000000000000000, -18.49999999999999645, 4.000000000000000000 ) ) ;
#20196 = FACE_OUTER_BOUND ( 'NONE', #248, .T. ) ;
#20197 = CARTESIAN_POINT ( 'NONE',  ( -13.84517967659089521, 2.744073667841084418, 6.715984435864265301 ) ) ;
#20198 = CARTESIAN_POINT ( 'NONE',  ( 11.96530858231679595, -20.22900456129164937, 4.174186261275266929 ) ) ;
#20199 = DIRECTION ( 'NONE',  ( 1.000000000000000000, 0.000000000000000000, 0.000000000000000000 ) ) ;
#20200 = ORIENTED_EDGE ( 'NONE', *, *, #11067, .F. ) ;
#20201 = ORIENTED_EDGE ( 'NONE', *, *, #19216, .T. ) ;
#20202 = CARTESIAN_POINT ( 'NONE',  ( 13.71569110726703045, -3.795099083046435506, 6.575359435862661250 ) ) ;
#20203 = CARTESIAN_POINT ( 'NONE',  ( 0.000000000000000000, 16.00000000000000000, 1.000000000000000000 ) ) ;
#20204 = ORIENTED_EDGE ( 'NONE', *, *, #17568, .T. ) ;
#20205 = EDGE_CURVE ( 'NONE', #4517, #1847, #7623, .T. ) ;
#20206 = CARTESIAN_POINT ( 'NONE',  ( -11.00000000000000000, -23.83493649053891517, 5.249999999999999112 ) ) ;
#20207 = ORIENTED_EDGE ( 'NONE', *, *, #3993, .F. ) ;
#20208 = CARTESIAN_POINT ( 'NONE',  ( -8.590308582316794173, -21.32581373872472597, 1.729004561291657582 ) ) ;
#20209 = CARTESIAN_POINT ( 'NONE',  ( 13.87215786865436762, 4.856472367046606564, 5.506273593909547515 ) ) ;
#20210 = DIRECTION ( 'NONE',  ( -1.000000000000000000, -0.000000000000000000, -0.000000000000000000 ) ) ;
#20211 = CARTESIAN_POINT ( 'NONE',  ( 1.126276606324276619, -8.364917468222230923, 1.622643865078341907 ) ) ;
#20212 = DIRECTION ( 'NONE',  ( -0.000000000000000000, -0.000000000000000000, -1.000000000000000000 ) ) ;
#20213 = CARTESIAN_POINT ( 'NONE',  ( -13.08439876642066935, 3.699637704240349656, 5.251001356674258602 ) ) ;
#20214 = CARTESIAN_POINT ( 'NONE',  ( 13.92791111847407848, 0.000000000000000000, 1.000000000000000000 ) ) ;
#20215 = CARTESIAN_POINT ( 'NONE',  ( -13.67732412376249052, -5.732631749971324631, 6.533692769198849781 ) ) ;
#20216 = DIRECTION ( 'NONE',  ( 0.000000000000000000, 1.000000000000000000, 0.000000000000000000 ) ) ;
#20217 = CARTESIAN_POINT ( 'NONE',  ( 4.687312169500634340, -21.70215802671379990, 4.455959925339818106 ) ) ;
#20218 = CARTESIAN_POINT ( 'NONE',  ( 5.034691417683178294, -20.22900456129164581, 2.825813738724747726 ) ) ;
#20219 = CARTESIAN_POINT ( 'NONE',  ( -8.309058582316792396, -23.27327832286945153, 2.298404588716537411 ) ) ;
#20220 = ORIENTED_EDGE ( 'NONE', *, *, #20205, .T. ) ;
#20221 = CARTESIAN_POINT ( 'NONE',  ( 13.09560269887985307, 4.265436293439658577, 4.973800642626965640 ) ) ;
#20222 = CARTESIAN_POINT ( 'NONE',  ( -32.65117217603048516, 6.460468870412185538, 1.000000000000000000 ) ) ;
#20223 = VERTEX_POINT ( 'NONE', #354 ) ;
#20224 = VERTEX_POINT ( 'NONE', #4952 ) ;
#20225 = CARTESIAN_POINT ( 'NONE',  ( -29.71062960567704891, 11.64110105645932691, -1.734723475976807094E-15 ) ) ;
#20226 = EDGE_CURVE ( 'NONE', #68, #9026, #1818, .T. ) ;
#20227 = CARTESIAN_POINT ( 'NONE',  ( -12.95145221759166354, -3.764163011652346569, 5.840524842913703552 ) ) ;
#20228 = AXIS2_PLACEMENT_3D ( 'NONE', #18477, #18681, #4348 ) ;
#20229 = CARTESIAN_POINT ( 'NONE',  ( -2.579281110863027582, -9.822567596814183233, 2.554382554832406615 ) ) ;
#20230 = CARTESIAN_POINT ( 'NONE',  ( -13.87470623115321899, 4.985164673244912414, 4.958488177337359026 ) ) ;
#20231 = EDGE_CURVE ( 'NONE', #11513, #2226, #5257, .T. ) ;
#20232 = DIRECTION ( 'NONE',  ( -0.000000000000000000, 1.000000000000000000, -0.000000000000000000 ) ) ;
#20233 = CARTESIAN_POINT ( 'NONE',  ( 26.79469207716614676, 9.000000000000001776, 1.000000000000000000 ) ) ;
#20234 = LINE ( 'NONE', #12064, #1020 ) ;
#20235 = EDGE_CURVE ( 'NONE', #14721, #12182, #20040, .T. ) ;
#20236 = CARTESIAN_POINT ( 'NONE',  ( 0.000000000000000000, 10.00000000000000000, 1.000000000000000000 ) ) ;
#20237 = CARTESIAN_POINT ( 'NONE',  ( 0.000000000000000000, -9.114917468222230923, 2.372643865078340575 ) ) ;
#20238 = CARTESIAN_POINT ( 'NONE',  ( -8.590308582316797725, -21.01515356694490322, 0.9790045612916562501 ) ) ;
#20239 = CARTESIAN_POINT ( 'NONE',  ( -0.5631383031621635116, -8.364917468222230923, 1.622643865078341907 ) ) ;
#20240 = ORIENTED_EDGE ( 'NONE', *, *, #2333, .T. ) ;
#20241 = CARTESIAN_POINT ( 'NONE',  ( -13.84501474873290938, 4.235744811019327649, 4.974109985360144037 ) ) ;
#20242 = DIRECTION ( 'NONE',  ( 0.000000000000000000, 1.000000000000000000, 0.000000000000000000 ) ) ;
#20243 = CARTESIAN_POINT ( 'NONE',  ( 12.15969141768317918, -22.98484643305507191, 0.9790045612916508100 ) ) ;
#20244 = CARTESIAN_POINT ( 'NONE',  ( -9.628441417683177406, -20.99999999999999645, 3.550687472877664952 ) ) ;
#20245 = ORIENTED_EDGE ( 'NONE', *, *, #6354, .T. ) ;
#20246 = CARTESIAN_POINT ( 'NONE',  ( 13.38795836133016870, -20.34560275282643005, 5.879540349057044146 ) ) ;
#20247 = FACE_OUTER_BOUND ( 'NONE', #15736, .T. ) ;
#20248 = ORIENTED_EDGE ( 'NONE', *, *, #14644, .F. ) ;
#20249 = EDGE_LOOP ( 'NONE', ( #11840, #7417, #19011, #16648 ) ) ;
#20250 = FACE_OUTER_BOUND ( 'NONE', #10448, .T. ) ;
#20251 = VERTEX_POINT ( 'NONE', #14780 ) ;
#20252 = CARTESIAN_POINT ( 'NONE',  ( -13.87470602645761986, 4.985154336109792972, 4.333333333333379223 ) ) ;
#20253 = ADVANCED_FACE ( 'NONE', ( #19404 ), #9768, .T. ) ;
#20254 = CARTESIAN_POINT ( 'NONE',  ( 1.513434189748285696, -9.114917468222230923, 2.372643865078341019 ) ) ;
#20255 = EDGE_LOOP ( 'NONE', ( #18397, #10590, #605, #7861 ) ) ;
#20256 = DIRECTION ( 'NONE',  ( 1.000000000000000000, -0.000000000000000000, 0.000000000000000000 ) ) ;
#20257 = CARTESIAN_POINT ( 'NONE',  ( 2.693754455098655409, -10.04853567022903782, 2.237415670251142519 ) ) ;
#20258 = LINE ( 'NONE', #5918, #20034 ) ;
#20259 = CARTESIAN_POINT ( 'NONE',  ( 3.486710468562268961, -9.848741751643258269, 2.003719583429115492 ) ) ;
#20260 = PLANE ( 'NONE',  #5227 ) ;
#20261 = VECTOR ( 'NONE', #1613, 1000.000000000000000 ) ;
#20262 = LINE ( 'NONE', #5921, #5748 ) ;
#20263 = LINE ( 'NONE', #1325, #2295 ) ;
#20264 = LINE ( 'NONE', #18691, #20075 ) ;
#20265 = CARTESIAN_POINT ( 'NONE',  ( 13.12529397354238192, 5.014845663890295846, 3.000000000000000000 ) ) ;
#20266 = CARTESIAN_POINT ( 'NONE',  ( 7.190941417683177406, -22.74294823697955081, 4.171265325393542334 ) ) ;
#20267 = CARTESIAN_POINT ( 'NONE',  ( -13.08094078691552831, 2.775009739235173356, 5.981149842915306714 ) ) ;
#20268 = ADVANCED_FACE ( 'NONE', ( #5365 ), #5062, .T. ) ;
#20269 = CARTESIAN_POINT ( 'NONE',  ( -8.121558582316795949, -22.99999999999999645, 3.550687472877652073 ) ) ;
#20270 = CARTESIAN_POINT ( 'NONE',  ( -7.659691417683177406, -22.98484643305507191, 0.9790045612916508100 ) ) ;
#20271 = VERTEX_POINT ( 'NONE', #6934 ) ;
#20272 = CARTESIAN_POINT ( 'NONE',  ( 12.62499999998404299, -19.49999999996810729, 2.793053905886972998 ) ) ;
#20273 = DIRECTION ( 'NONE',  ( -0.000000000000000000, -0.000000000000000000, -1.000000000000000000 ) ) ;
#20274 = ORIENTED_EDGE ( 'NONE', *, *, #15949, .T. ) ;
#20275 = VECTOR ( 'NONE', #15371, 1000.000000000000000 ) ;
#20276 = DIRECTION ( 'NONE',  ( 0.000000000000000000, -1.000000000000000000, 0.000000000000000000 ) ) ;
#20277 = ORIENTED_EDGE ( 'NONE', *, *, #7472, .F. ) ;
#20278 = CARTESIAN_POINT ( 'NONE',  ( 2.875042468481914248, -11.91375063635796039, 3.091440134965714126 ) ) ;
#20279 = ADVANCED_FACE ( 'NONE', ( #2224 ), #9866, .T. ) ;
#20280 = EDGE_CURVE ( 'NONE', #16495, #16469, #19299, .T. ) ;
#20281 = ORIENTED_EDGE ( 'NONE', *, *, #16428, .F. ) ;
#20282 = DIRECTION ( 'NONE',  ( 1.000000000000000000, 0.000000000000000000, -0.000000000000000000 ) ) ;
#20283 = CYLINDRICAL_SURFACE ( 'NONE', #280, 10.00000000000000000 ) ;
#20284 = CARTESIAN_POINT ( 'NONE',  ( -2.088806020750596737, -10.42712783963456857, 1.767030719737609168 ) ) ;
#20285 = DIRECTION ( 'NONE',  ( -0.000000000000000000, 1.304178812473495102E-15, 1.000000000000000000 ) ) ;
#20286 = PLANE ( 'NONE',  #17377 ) ;
#20287 = CARTESIAN_POINT ( 'NONE',  ( -10.38119784648305632, -14.00000000000000000, 1.000000000000000000 ) ) ;
#20288 = CARTESIAN_POINT ( 'NONE',  ( 11.50344141768317741, -22.05068747287766229, 6.000000000000001776 ) ) ;
#20289 = CARTESIAN_POINT ( 'NONE',  ( -13.10431844137356627, 3.955581289335645234, 6.006545679920360925 ) ) ;
#20290 = EDGE_CURVE ( 'NONE', #10647, #16179, #8413, .T. ) ;
#20291 = CARTESIAN_POINT ( 'NONE',  ( -11.87844141768317563, -23.74999999999999645, 3.449312527122335492 ) ) ;
#20292 = VERTEX_POINT ( 'NONE', #457 ) ;
#20293 = CARTESIAN_POINT ( 'NONE',  ( 12.71530858231679240, -23.77099543870833998, 2.825813738724734847 ) ) ;
#20294 = CARTESIAN_POINT ( 'NONE',  ( -7.499999999999999112, -18.49999999999999645, 6.500000000000000888 ) ) ;
#20295 = CARTESIAN_POINT ( 'NONE',  ( -13.37505392270939986, -20.99727690317663686, 4.612442573673130930 ) ) ;
#20296 = CARTESIAN_POINT ( 'NONE',  ( 11.59030858231679417, -21.32581373872472597, 1.729004561291657582 ) ) ;
#20297 = LINE ( 'NONE', #12330, #17003 ) ;
#20298 = ORIENTED_EDGE ( 'NONE', *, *, #20136, .T. ) ;
#20299 = ORIENTED_EDGE ( 'NONE', *, *, #13739, .T. ) ;
#20300 = CARTESIAN_POINT ( 'NONE',  ( 13.40432071140796744, -19.51930407389869515, 6.223619713037471968 ) ) ;
#20301 = CARTESIAN_POINT ( 'NONE',  ( 21.67243175760212637, 9.000000000000001776, 1.000000000000000000 ) ) ;
#20302 = ORIENTED_EDGE ( 'NONE', *, *, #11779, .F. ) ;
#20303 = LINE ( 'NONE', #5964, #114 ) ;
#20304 = VERTEX_POINT ( 'NONE', #13301 ) ;
#20305 = CARTESIAN_POINT ( 'NONE',  ( -12.90280858231679773, -22.77556120703056308, 1.770995438708339975 ) ) ;
#20306 = FACE_OUTER_BOUND ( 'NONE', #15832, .T. ) ;
#20307 = DIRECTION ( 'NONE',  ( 0.000000000000000000, -0.2487476929738665354, -0.9685683172808094987 ) ) ;
#20308 = CARTESIAN_POINT ( 'NONE',  ( 1.948765222931501784, -9.143197003266354983, 1.629906614618163552 ) ) ;
#20309 = AXIS2_PLACEMENT_3D ( 'NONE', #7842, #20612, #4804 ) ;
#20310 = CARTESIAN_POINT ( 'NONE',  ( 17.12779268661489596, 0.000000000000000000, 1.000000000000000000 ) ) ;
#20311 = CARTESIAN_POINT ( 'NONE',  ( -13.37499994994395891, -19.50000252782794519, 4.474109982178703149 ) ) ;
#20312 = CARTESIAN_POINT ( 'NONE',  ( 11.12155858231679417, -23.74999999999999645, 3.550687472877651629 ) ) ;
#20313 = CARTESIAN_POINT ( 'NONE',  ( -13.41115317570721110, -19.17426462678482579, 6.244630269197427808 ) ) ;
#20314 = EDGE_CURVE ( 'NONE', #10279, #2639, #11539, .T. ) ;
#20315 = LINE ( 'NONE', #14433, #8045 ) ;
#20316 = CARTESIAN_POINT ( 'NONE',  ( 5.027808582316795949, -22.97900456129165647, 3.964901035250747885 ) ) ;
#20317 = VECTOR ( 'NONE', #4703, 1000.000000000000000 ) ;
#20318 = CARTESIAN_POINT ( 'NONE',  ( 9.815941417683177406, -21.32873467460645145, 4.242948236979555254 ) ) ;
#20319 = CARTESIAN_POINT ( 'NONE',  ( -6.809058582316794173, -23.27327832286945153, 2.298404588716537411 ) ) ;
#20320 = VERTEX_POINT ( 'NONE', #8507 ) ;
#20321 = CARTESIAN_POINT ( 'NONE',  ( 13.09560264576187905, 4.265433610975056133, 4.916666666666649199 ) ) ;
#20322 = CARTESIAN_POINT ( 'NONE',  ( -1.948765222931501784, -9.143197003266354983, 1.629906614618163552 ) ) ;
#20323 = ORIENTED_EDGE ( 'NONE', *, *, #1099, .F. ) ;
#20324 = VECTOR ( 'NONE', #19553, 1000.000000000000000 ) ;
#20325 = ORIENTED_EDGE ( 'NONE', *, *, #7932, .T. ) ;
#20326 = DIRECTION ( 'NONE',  ( -0.000000000000000000, -0.000000000000000000, -1.000000000000000000 ) ) ;
#20327 = PRODUCT_DEFINITION ( 'UNKNOWN', '', #12374, #15905 ) ;
#20328 = CARTESIAN_POINT ( 'NONE',  ( -13.10624331898488037, 4.052787608736739600, 6.006964772046813117 ) ) ;
#20329 = CARTESIAN_POINT ( 'NONE',  ( -2.203959450683124377, -9.262433282444222371, 2.410528873095051594 ) ) ;
#20330 = CARTESIAN_POINT ( 'NONE',  ( -13.87066368810231154, 4.781016249162736820, 5.617237349937618696 ) ) ;
#20331 = CARTESIAN_POINT ( 'NONE',  ( 6.183390479346035917, 9.000000000000001776, 1.000000000000000000 ) ) ;
#20332 = DIRECTION ( 'NONE',  ( 0.000000000000000000, 0.000000000000000000, 1.000000000000000000 ) ) ;
#20333 = LINE ( 'NONE', #10816, #15375 ) ;
#20334 = DIRECTION ( 'NONE',  ( -0.000000000000000000, -0.000000000000000000, -1.000000000000000000 ) ) ;
#20335 =( BOUNDED_CURVE ( )  B_SPLINE_CURVE ( 2, ( #11264, #14287, #14505, #3319, #17758, #9591, #3427, #4786, #1757, #12622, #8143, #3219, #15867, #15967, #7923, #12930, #183, #14190, #1856, #6671, #8034, #13042, #17542, #1651, #11171, #14402, #11074, #8240, #5098, #85, #6248, #20700, #9700, #19027, #6567, #1545, #19134, #4681, #9805, #19333, #19443, #16191, #14604, #279, #11479, #17859, #9904, #17443, #6363, #16285, #7827, #5405, #803, #2258, #10429, #11671, #15127, #11575, #11777, #393, #3834, #8644, #8338, #18169, #699, #15018, #16386, #10318, #10213, #13346, #13550, #5504, #7186, #8543, #19951, #16687, #19747, #8756, #6872, #590, #13449, #13239, #1956, #14716, #19638, #5295, #5609, #6776, #3624, #16580, #16488, #11981, #10008, #7085, #19853 ),
 .UNSPECIFIED., .F., .F. ) 
 B_SPLINE_CURVE_WITH_KNOTS ( ( 3, 2, 2, 2, 2, 2, 2, 2, 2, 2, 2, 2, 2, 2, 2, 2, 2, 2, 2, 2, 2, 2, 2, 2, 2, 2, 2, 2, 2, 2, 2, 2, 2, 2, 2, 2, 2, 2, 2, 2, 2, 2, 2, 2, 2, 2, 2, 3 ),
 ( 0.000000000000000000, 0.02083333333333333218, 0.04166666666666666435, 0.06250000000000000000, 0.08333333333333332871, 0.1041666666666666713, 0.1250000000000000000, 0.1458333333333333426, 0.1666666666666666574, 0.1875000000000000000, 0.2083333333333333426, 0.2291666666666666574, 0.2500000000000000000, 0.2708333333333333148, 0.2916666666666666852, 0.3124999999999999445, 0.3333333333333333148, 0.3541666666666666852, 0.3750000000000000000, 0.3958333333333333148, 0.4166666666666666852, 0.4375000000000000555, 0.4583333333333333148, 0.4791666666666666852, 0.5000000000000000000, 0.5208333333333333703, 0.5416666666666666297, 0.5625000000000000000, 0.5833333333333333703, 0.6041666666666666297, 0.6249999999999998890, 0.6458333333333333703, 0.6666666666666666297, 0.6875000000000000000, 0.7083333333333333703, 0.7291666666666666297, 0.7500000000000000000, 0.7708333333333333703, 0.7916666666666666297, 0.8125000000000000000, 0.8333333333333333703, 0.8541666666666666297, 0.8750000000000001110, 0.8958333333333333703, 0.9166666666666666297, 0.9375000000000000000, 0.9583333333333333703, 0.9650437087885355147 ),
 .UNSPECIFIED. ) 
 CURVE ( )  GEOMETRIC_REPRESENTATION_ITEM ( )  RATIONAL_B_SPLINE_CURVE ( ( 1.000000000000000000, 0.9238795325112867385, 1.000000000000000000, 0.9238795325112867385, 1.000000000000000000, 0.9238795325112867385, 1.000000000000000000, 0.9238795325112867385, 1.000000000000000000, 0.9238795325112867385, 1.000000000000000000, 0.9238795325112867385, 1.000000000000000000, 0.9238795325112867385, 1.000000000000000000, 0.9238795325112867385, 1.000000000000000000, 0.9238795325112867385, 1.000000000000000000, 0.9238795325112867385, 1.000000000000000000, 0.9238795325112867385, 1.000000000000000000, 0.9238795325112867385, 1.000000000000000000, 0.9238795325112867385, 1.000000000000000000, 0.9238795325112867385, 1.000000000000000000, 0.9238795325112867385, 1.000000000000000000, 0.9238795325112867385, 1.000000000000000000, 0.9238795325112867385, 1.000000000000000000, 0.9238795325112867385, 1.000000000000000000, 0.9238795325112867385, 1.000000000000000000, 0.9238795325112867385, 1.000000000000000000, 0.9238795325112867385, 1.000000000000000000, 0.9238795325112867385, 1.000000000000000000, 0.9238795325112867385, 1.000000000000000000, 0.9238795325112867385, 1.000000000000000000, 0.9238795325112867385, 1.000000000000000000, 0.9238795325112867385, 1.000000000000000000, 0.9238795325112867385, 1.000000000000000000, 0.9238795325112867385, 1.000000000000000000, 0.9238795325112867385, 1.000000000000000000, 0.9238795325112867385, 1.000000000000000000, 0.9238795325112867385, 1.000000000000000000, 0.9238795325112867385, 1.000000000000000000, 0.9238795325112867385, 1.000000000000000000, 0.9238795325112867385, 1.000000000000000000, 0.9238795325112867385, 1.000000000000000000, 0.9238795325112867385, 1.000000000000000000, 0.9238795325112867385, 1.000000000000000000, 0.9238795325112867385, 1.000000000000000000, 0.9238795325112867385, 1.000000000000000000, 0.9238795325112867385, 1.000000000000000000, 0.9238795325112867385, 1.000000000000000000, 0.9238795325112867385, 1.000000000000000000, 0.9238795325112867385, 1.000000000000000000, 0.9238795325112867385, 1.000000000000000000, 0.9238795325112867385, 1.000000000000000000, 0.9238795325112867385, 1.000000000000000000, 0.9754817479996107377, 0.9667580569362973497 ) ) 
 REPRESENTATION_ITEM ( '' )  );
#20336 = DIRECTION ( 'NONE',  ( 0.000000000000000000, 1.000000000000000000, 0.000000000000000000 ) ) ;
#20337 = CARTESIAN_POINT ( 'NONE',  ( -7.934058582316796837, -23.73192549717337130, 5.303608408759367343 ) ) ;
#20338 = CARTESIAN_POINT ( 'NONE',  ( 0.000000000000000000, -9.114917468222230923, 1.622643865078341019 ) ) ;
#20339 = ORIENTED_EDGE ( 'NONE', *, *, #7457, .T. ) ;
#20340 = CARTESIAN_POINT ( 'NONE',  ( -13.84501469867365131, 4.235742283194553259, 3.333333333332063386 ) ) ;
#20341 = LINE ( 'NONE', #18561, #17056 ) ;
#20342 = CARTESIAN_POINT ( 'NONE',  ( 12.25344141768317741, -21.94931252712233061, 0.9999999999999978906 ) ) ;
#20343 = CARTESIAN_POINT ( 'NONE',  ( -13.37155858231679595, -20.99999999999999645, 3.449312527122348371 ) ) ;
#20344 = ORIENTED_EDGE ( 'NONE', *, *, #5170, .T. ) ;
#20345 = CARTESIAN_POINT ( 'NONE',  ( 13.87467358130843387, 4.983515856073828409, 5.065827972856573602 ) ) ;
#20346 = DIRECTION ( 'NONE',  ( -0.000000000000000000, -0.000000000000000000, -1.000000000000000000 ) ) ;
#20347 = CIRCLE ( 'NONE', #15983, 0.4999999999999987232 ) ;
#20348 = ORIENTED_EDGE ( 'NONE', *, *, #20017, .T. ) ;
#20349 = ORIENTED_EDGE ( 'NONE', *, *, #7997, .T. ) ;
#20350 = DIRECTION ( 'NONE',  ( 1.000000000000000000, 0.000000000000000000, 0.000000000000000000 ) ) ;
#20351 = VECTOR ( 'NONE', #17004, 1000.000000000000000 ) ;
#20352 = ORIENTED_EDGE ( 'NONE', *, *, #14564, .F. ) ;
#20353 = FACE_OUTER_BOUND ( 'NONE', #5628, .T. ) ;
#20354 = EDGE_CURVE ( 'NONE', #3944, #2453, #11439, .T. ) ;
#20355 = EDGE_CURVE ( 'NONE', #8228, #10614, #8537, .T. ) ;
#20356 = VECTOR ( 'NONE', #18602, 1000.000000000000000 ) ;
#20357 = CARTESIAN_POINT ( 'NONE',  ( 2.436080212393455735, -9.483920418190111334, 2.467411194204634839 ) ) ;
#20358 = ORIENTED_EDGE ( 'NONE', *, *, #6760, .T. ) ;
#20359 = LINE ( 'NONE', #18375, #20701 ) ;
#20360 = DIRECTION ( 'NONE',  ( -1.000000000000000000, 0.000000000000000000, 0.000000000000000000 ) ) ;
#20361 = DIRECTION ( 'NONE',  ( -1.000000000000000000, -0.000000000000000000, -0.000000000000000000 ) ) ;
#20362 = AXIS2_PLACEMENT_3D ( 'NONE', #1826, #17616, #8112 ) ;
#20363 = CARTESIAN_POINT ( 'NONE',  ( 2.012076196476103362, -9.160103213191565175, 1.634248467062433541 ) ) ;
#20364 = DIRECTION ( 'NONE',  ( 1.000000000000000000, 0.000000000000000000, 0.000000000000000000 ) ) ;
#20365 = CIRCLE ( 'NONE', #17327, 1.499999999999998668 ) ;
#20366 = CARTESIAN_POINT ( 'NONE',  ( 13.10821839766814279, 4.152529082241303904, 5.997503362667785609 ) ) ;
#20367 = VECTOR ( 'NONE', #20199, 1000.000000000000000 ) ;
#20368 = CARTESIAN_POINT ( 'NONE',  ( -4.250698171653726654, 0.000000000000000000, 0.000000000000000000 ) ) ;
#20369 = LINE ( 'NONE', #17423, #12724 ) ;
#20370 = CARTESIAN_POINT ( 'NONE',  ( -3.999999999999999112, -7.500000000000047073, 9.999999999999998224 ) ) ;
#20371 = CARTESIAN_POINT ( 'NONE',  ( 4.940941417683177406, -21.25705176302044208, 2.828734674606458555 ) ) ;
#20372 = CARTESIAN_POINT ( 'NONE',  ( -13.12529397354238192, 5.014845663890295846, 4.166666666666765551 ) ) ;
#20373 = CARTESIAN_POINT ( 'NONE',  ( -7.840308582316795949, -22.36352608949544418, 4.520995438708343528 ) ) ;
#20374 = EDGE_CURVE ( 'NONE', #9634, #4496, #18135, .T. ) ;
#20375 = CARTESIAN_POINT ( 'NONE',  ( -7.472191417683177406, -24.47900456129165292, 2.413778621189595963 ) ) ;
#20376 = ORIENTED_EDGE ( 'NONE', *, *, #9359, .T. ) ;
#20377 = CARTESIAN_POINT ( 'NONE',  ( 13.37500003877585186, -19.49999804181952712, 4.520055687292853008 ) ) ;
#20378 = FACE_OUTER_BOUND ( 'NONE', #16427, .T. ) ;
#20379 = VERTEX_POINT ( 'NONE', #11843 ) ;
#20380 = LINE ( 'NONE', #6350, #15300 ) ;
#20381 = EDGE_LOOP ( 'NONE', ( #1053, #6067, #8207, #8508 ) ) ;
#20382 = CARTESIAN_POINT ( 'NONE',  ( 2.602174906157317835, -9.976397331638239052, 2.593889103792902606 ) ) ;
#20383 = EDGE_CURVE ( 'NONE', #19224, #13004, #15394, .T. ) ;
#20384 = CIRCLE ( 'NONE', #13002, 10.00000000000000000 ) ;
#20385 = EDGE_CURVE ( 'NONE', #12897, #9608, #15286, .T. ) ;
#20386 = VECTOR ( 'NONE', #13611, 1000.000000000000000 ) ;
#20387 = VECTOR ( 'NONE', #17839, 1000.000000000000000 ) ;
#20388 = ORIENTED_EDGE ( 'NONE', *, *, #1652, .T. ) ;
#20389 = DIRECTION ( 'NONE',  ( 0.000000000000000000, 0.000000000000000000, 1.000000000000000000 ) ) ;
#20390 = LINE ( 'NONE', #15456, #13306 ) ;
#20391 = VECTOR ( 'NONE', #1623, 1000.000000000000000 ) ;
#20392 = CARTESIAN_POINT ( 'NONE',  ( -1.797685059409938280, -9.880079706704160358, 1.626537830816663588 ) ) ;
#20393 = PLANE ( 'NONE',  #8990 ) ;
#20394 = DIRECTION ( 'NONE',  ( -8.673617379884047798E-17, 1.000000000000000000, -0.000000000000000000 ) ) ;
#20395 = AXIS2_PLACEMENT_3D ( 'NONE', #12372, #10598, #20028 ) ;
#20396 = CARTESIAN_POINT ( 'NONE',  ( 4.472191417683178294, -24.47900456129165292, 2.413778621189595963 ) ) ;
#20397 = CARTESIAN_POINT ( 'NONE',  ( -9.689245429134309973, 10.00000000000000000, 1.000000000000000000 ) ) ;
#20398 = CARTESIAN_POINT ( 'NONE',  ( -12.34719141768317563, -21.22443879296941915, 1.770995438708345748 ) ) ;
#20399 = ADVANCED_FACE ( 'NONE', ( #766 ), #18645, .T. ) ;
#20400 = ORIENTED_EDGE ( 'NONE', *, *, #12042, .T. ) ;
#20401 = CARTESIAN_POINT ( 'NONE',  ( 5.121558582316794173, -23.74999999999999645, 3.550687472877651629 ) ) ;
#20402 = DIRECTION ( 'NONE',  ( 1.000000000000000000, 0.000000000000000000, -0.000000000000000000 ) ) ;
#20403 = CARTESIAN_POINT ( 'NONE',  ( -12.62608183053121458, -20.94536755816881168, 4.949360998036265613 ) ) ;
#20404 = ORIENTED_EDGE ( 'NONE', *, *, #2791, .T. ) ;
#20405 = CIRCLE ( 'NONE', #14362, 10.00000000000000000 ) ;
#20406 = CARTESIAN_POINT ( 'NONE',  ( 5.309058582316794173, -23.27327832286945153, 2.298404588716537411 ) ) ;
#20407 = CARTESIAN_POINT ( 'NONE',  ( 13.50000000000000178, 7.806255641895631925E-15, 2.000000000000000000 ) ) ;
#20408 = VERTEX_POINT ( 'NONE', #16759 ) ;
#20409 = ORIENTED_EDGE ( 'NONE', *, *, #7758, .F. ) ;
#20410 = CARTESIAN_POINT ( 'NONE',  ( 13.37500027835944039, -20.99998594284889464, 4.544258551573043370 ) ) ;
#20411 = DIRECTION ( 'NONE',  ( 1.000000000000000000, 0.000000000000000000, 0.000000000000000000 ) ) ;
#20412 = SURFACE_SIDE_STYLE ('',( #12337 ) ) ;
#20413 = ORIENTED_EDGE ( 'NONE', *, *, #4749, .T. ) ;
#20414 = CARTESIAN_POINT ( 'NONE',  ( -0.000000000000000000, 11.64110105645932691, 0.000000000000000000 ) ) ;
#20415 = VERTEX_POINT ( 'NONE', #5784 ) ;
#20416 = EDGE_CURVE ( 'NONE', #8358, #13991, #12153, .T. ) ;
#20417 = CARTESIAN_POINT ( 'NONE',  ( -11.30905858231679417, -23.27327832286945153, 2.298404588716537411 ) ) ;
#20418 = DIRECTION ( 'NONE',  ( -1.000000000000000000, -5.782411586589356653E-16, 0.000000000000000000 ) ) ;
#20419 = CARTESIAN_POINT ( 'NONE',  ( -4.687312169500630787, -21.51559725698340131, 5.182386163300424009 ) ) ;
#20420 = FACE_OUTER_BOUND ( 'NONE', #14099, .T. ) ;
#20421 = CARTESIAN_POINT ( 'NONE',  ( 0.9854920305337622199, -8.364917468222230923, 1.622643865078341907 ) ) ;
#20422 = VECTOR ( 'NONE', #20346, 1000.000000000000000 ) ;
#20423 = AXIS2_PLACEMENT_3D ( 'NONE', #15614, #7787, #8935 ) ;
#20424 = AXIS2_PLACEMENT_3D ( 'NONE', #6615, #9752, #15815 ) ;
#20425 = CARTESIAN_POINT ( 'NONE',  ( 2.499999999999998668, -19.50000000000000000, 4.000000000000000000 ) ) ;
#20426 = CARTESIAN_POINT ( 'NONE',  ( -13.09494140422671471, 4.232040913449062636, 5.131376921800749003 ) ) ;
#20427 = CARTESIAN_POINT ( 'NONE',  ( 5.496558582316794173, -22.05068747287764452, 1.749999999999998446 ) ) ;
#20428 = CARTESIAN_POINT ( 'NONE',  ( -12.63806878948643231, -20.34002613093225520, 5.891296472647073124 ) ) ;
#20429 = EDGE_CURVE ( 'NONE', #6686, #6562, #10387, .T. ) ;
#20430 = EDGE_CURVE ( 'NONE', #4871, #4902, #8918, .T. ) ;
#20431 = DIRECTION ( 'NONE',  ( 1.000000000000000000, 0.000000000000000000, 0.000000000000000000 ) ) ;
#20432 = CARTESIAN_POINT ( 'NONE',  ( 6.434058582316796837, -22.67126532539354855, 4.242948236979545484 ) ) ;
#20433 = CARTESIAN_POINT ( 'NONE',  ( 11.69094141768317741, -22.74294823697955081, 4.171265325393542334 ) ) ;
#20434 = CARTESIAN_POINT ( 'NONE',  ( -4.934058582316793284, -23.20159541128345992, 4.773278322869455970 ) ) ;
#20435 = ORIENTED_EDGE ( 'NONE', *, *, #4630, .F. ) ;
#20436 = CARTESIAN_POINT ( 'NONE',  ( 13.09560264576187905, 4.265433610975056133, 4.166666666666765551 ) ) ;
#20437 = AXIS2_PLACEMENT_3D ( 'NONE', #16418, #14538, #9733 ) ;
#20438 = CYLINDRICAL_SURFACE ( 'NONE', #8335, 10.00000000000000000 ) ;
#20439 = ORIENTED_EDGE ( 'NONE', *, *, #9585, .F. ) ;
#20440 = CIRCLE ( 'NONE', #11396, 2.500000000000000444 ) ;
#20441 = EDGE_LOOP ( 'NONE', ( #20245, #1604, #3236, #18181, #20172, #7414 ) ) ;
#20442 = DIRECTION ( 'NONE',  ( -0.000000000000000000, -0.000000000000000000, -1.000000000000000000 ) ) ;
#20443 = EDGE_CURVE ( 'NONE', #12487, #9838, #15690, .T. ) ;
#20444 = CARTESIAN_POINT ( 'NONE',  ( -12.64131715375063258, -19.42598373559290792, 5.491151580003103660 ) ) ;
#20445 = CARTESIAN_POINT ( 'NONE',  ( -3.034277558025862298, -9.029550313327863620, 2.543334857076493094 ) ) ;
#20446 = CARTESIAN_POINT ( 'NONE',  ( -13.87454419214980739, 4.976981703567351367, 5.131312659523921127 ) ) ;
#20447 = DIRECTION ( 'NONE',  ( -0.000000000000000000, 0.000000000000000000, 1.000000000000000000 ) ) ;
#20448 = CARTESIAN_POINT ( 'NONE',  ( -11.00000000000000000, -20.16506350946107418, 5.000000000000000000 ) ) ;
#20449 = DIRECTION ( 'NONE',  ( 1.000000000000000000, -0.000000000000000000, -0.000000000000000000 ) ) ;
#20450 = DIRECTION ( 'NONE',  ( 0.000000000000000000, 1.000000000000000000, 0.000000000000000000 ) ) ;
#20451 = VECTOR ( 'NONE', #8682, 1000.000000000000000 ) ;
#20452 = CARTESIAN_POINT ( 'NONE',  ( -11.12155858231679595, -24.50000000000000000, 3.550687472877651629 ) ) ;
#20453 = CARTESIAN_POINT ( 'NONE',  ( -2.309828811027716977, -9.292785183284841821, 1.668323847571005603 ) ) ;
#20454 = VERTEX_POINT ( 'NONE', #7353 ) ;
#20455 = CARTESIAN_POINT ( 'NONE',  ( -13.84402619238587206, 4.185822715484293077, 5.150938132831436533 ) ) ;
#20456 = LINE ( 'NONE', #4333, #13053 ) ;
#20457 = CARTESIAN_POINT ( 'NONE',  ( 5.215308582316795949, -24.52099543870834708, 2.515153566944913432 ) ) ;
#20458 = CARTESIAN_POINT ( 'NONE',  ( -12.34030858231679773, -22.36352608949544418, 4.520995438708343528 ) ) ;
#20459 = EDGE_LOOP ( 'NONE', ( #17943, #18913, #4369, #17873 ) ) ;
#20460 = CARTESIAN_POINT ( 'NONE',  ( 13.37500000000002132, -21.00000000000274269, 4.083333333315724012 ) ) ;
#20461 = LINE ( 'NONE', #13844, #367 ) ;
#20462 = ORIENTED_EDGE ( 'NONE', *, *, #27, .T. ) ;
#20463 = VERTEX_POINT ( 'NONE', #10589 ) ;
#20464 = DIRECTION ( 'NONE',  ( -0.000000000000000000, -0.000000000000000000, -1.000000000000000000 ) ) ;
#20465 = EDGE_LOOP ( 'NONE', ( #18954, #18759, #3134, #324 ) ) ;
#20466 = CARTESIAN_POINT ( 'NONE',  ( -13.86106797245302147, 4.296432608878145487, 5.947261916831099171 ) ) ;
#20467 = AXIS2_PLACEMENT_3D ( 'NONE', #3283, #6321, #7893 ) ;
#20468 = EDGE_CURVE ( 'NONE', #12772, #20175, #8822, .T. ) ;
#20469 = CARTESIAN_POINT ( 'NONE',  ( 1.797604806073912709, -9.120796646272857799, 2.374153755450133740 ) ) ;
#20470 = VERTEX_POINT ( 'NONE', #20015 ) ;
#20471 = CARTESIAN_POINT ( 'NONE',  ( -4.121804964265448845, -21.67354536559615497, 4.877507451124815319 ) ) ;
#20472 = EDGE_CURVE ( 'NONE', #3752, #1149, #15189, .T. ) ;
#20473 =( BOUNDED_SURFACE ( )  B_SPLINE_SURFACE ( 3, 3, ( 
 ( #11348, #19422, #6231, #1626, #1737, #14486, #8220, #6449, #19003, #6338, #5079, #12710, #12813, #3200, #17624, #4659, #9572, #15945, #14583, #9785, #1525, #3294, #11150, #6647, #11051, #17740, #19112, #8007, #17424, #16171, #11455, #258, #4765, #16064, #8119, #12910, #3404, #373, #14892, #5485 ),
 ( #7063, #2341, #10093, #8735, #18250, #571, #10293, #1933, #16562, #8429, #5175, #11651, #9883, #17934, #11858, #11554, #16468, #13125, #8625, #475, #2237, #3913, #2141, #18042, #3603, #6849, #6951, #19617, #9983, #16663, #3715, #16365, #19522, #11758, #13322, #15103, #780, #8523, #14796, #2043 ),
 ( #7166, #19722, #13219, #5275, #5383, #18149, #3814, #11959, #6756, #10192, #14994, #19832, #675, #13426, #3504, #13529, #19931, #5588, #16265, #8316, #14691, #4222, #13625, #10821, #4019, #16874, #15512, #10602, #16976, #880, #12170, #1294, #2444, #15412, #13735, #18558, #7673, #20239, #9239, #18772 ),
 ( #15303, #14043, #8932, #2653, #9040, #5897, #10404, #1095, #7475, #2864, #4437, #12070, #13834, #20139, #15611, #16775, #7573, #2544, #5799, #8836, #17186, #20453, #6110, #20033, #18355, #12267, #13935, #7264, #18661, #10712, #15204, #4329, #5695, #18460, #17086, #2764, #4123, #9142, #1194, #20338 ),
 ( #10504, #6002, #982, #7371, #12377, #11023, #9649, #19081, #4738, #15718, #6306, #16142, #17281, #9548, #7880, #12678, #1809, #14350, #3378, #12886, #8094, #12785, #8194, #33, #4942, #6205, #18873, #14560, #14459, #3271, #17392, #4534, #16033, #1597, #11322, #17494, #14240, #9450, #2966, #11124 ),
 ( #19289, #9759, #17707, #7784, #233, #20647, #139, #1402, #3174, #4841, #10919, #15919, #9342, #12480, #7976, #19187, #14147, #6422, #11222, #17598, #12574, #6523, #1710, #20554, #18975, #4629, #3075, #15821, #1499, #648, #3686, #13404, #5052, #19694, #11529, #8291, #14772, #12992, #345, #14968 ),
 ( #6924, #2215, #13097, #449, #19810, #14665, #10070, #14870, #16341, #5358, #7036, #2015, #16445, #11735, #6827, #11836, #2118, #3889, #2315, #8705, #13197, #6729, #19499, #5152, #8500, #5464, #19594, #17910, #8405, #5248, #11626, #546, #15076, #9856, #9958, #16241, #8598, #13294, #18128, #6622 ) ),
 .UNSPECIFIED., .T., .F., .T. ) 
 B_SPLINE_SURFACE_WITH_KNOTS ( ( 4, 3, 4 ),
 ( 4, 2, 2, 2, 2, 2, 2, 2, 2, 2, 2, 2, 2, 2, 2, 2, 2, 2, 2, 4 ),
 ( 0.000000000000000000, 0.5000000000000000000, 1.000000000000000000 ),
 ( 0.000000000000000000, 0.3100443560520446118, 0.4650665340780669177, 0.5425776230910780429, 0.5813331675975836887, 0.6007109398508364562, 0.6200887121040892236, 0.6309950902025724950, 0.6419014683010558775, 0.6637142244980225314, 0.7073397368919559502, 0.7509652492858893691, 0.7727780054828560230, 0.7836843835813394055, 0.7945907616798226769, 0.8074288390748337596, 0.8202669164698448423, 0.8459430712598670077, 0.8972953808399113385, 1.000000000000000000 ),
 .UNSPECIFIED. ) 
 GEOMETRIC_REPRESENTATION_ITEM ( )  RATIONAL_B_SPLINE_SURFACE ( (
 ( 1.000000000000000000, 1.000000000000000000, 1.000000000000000000, 1.000000000000000000, 1.000000000000000000, 1.000000000000000000, 1.000000000000000000, 1.000000000000000000, 1.000000000000000000, 1.000000000000000000, 1.000000000000000000, 1.000000000000000000, 1.000000000000000000, 1.000000000000000000, 1.000000000000000000, 1.000000000000000000, 1.000000000000000000, 1.000000000000000000, 1.000000000000000000, 1.000000000000000000, 1.000000000000000000, 1.000000000000000000, 1.000000000000000000, 1.000000000000000000, 1.000000000000000000, 1.000000000000000000, 1.000000000000000000, 1.000000000000000000, 1.000000000000000000, 1.000000000000000000, 1.000000000000000000, 1.000000000000000000, 1.000000000000000000, 1.000000000000000000, 1.000000000000000000, 1.000000000000000000, 1.000000000000000000, 1.000000000000000000, 1.000000000000000000, 1.000000000000000000),
 ( 0.3333333333333333703, 0.3333333333333333703, 0.3333333333333333703, 0.3333333333333333703, 0.3333333333333333703, 0.3333333333333333703, 0.3333333333333333703, 0.3333333333333333703, 0.3333333333333333703, 0.3333333333333333703, 0.3333333333333333703, 0.3333333333333333703, 0.3333333333333333703, 0.3333333333333333703, 0.3333333333333333703, 0.3333333333333333703, 0.3333333333333333703, 0.3333333333333333703, 0.3333333333333333703, 0.3333333333333333703, 0.3333333333333333703, 0.3333333333333333703, 0.3333333333333333703, 0.3333333333333333703, 0.3333333333333333703, 0.3333333333333333703, 0.3333333333333333703, 0.3333333333333333703, 0.3333333333333333703, 0.3333333333333333703, 0.3333333333333333703, 0.3333333333333333703, 0.3333333333333333703, 0.3333333333333333703, 0.3333333333333333703, 0.3333333333333333703, 0.3333333333333333703, 0.3333333333333333703, 0.3333333333333333703, 0.3333333333333333703),
 ( 0.3333333333333333703, 0.3333333333333333703, 0.3333333333333333703, 0.3333333333333333703, 0.3333333333333333703, 0.3333333333333333703, 0.3333333333333333703, 0.3333333333333333703, 0.3333333333333333703, 0.3333333333333333703, 0.3333333333333333703, 0.3333333333333333703, 0.3333333333333333703, 0.3333333333333333703, 0.3333333333333333703, 0.3333333333333333703, 0.3333333333333333703, 0.3333333333333333703, 0.3333333333333333703, 0.3333333333333333703, 0.3333333333333333703, 0.3333333333333333703, 0.3333333333333333703, 0.3333333333333333703, 0.3333333333333333703, 0.3333333333333333703, 0.3333333333333333703, 0.3333333333333333703, 0.3333333333333333703, 0.3333333333333333703, 0.3333333333333333703, 0.3333333333333333703, 0.3333333333333333703, 0.3333333333333333703, 0.3333333333333333703, 0.3333333333333333703, 0.3333333333333333703, 0.3333333333333333703, 0.3333333333333333703, 0.3333333333333333703),
 ( 1.000000000000000000, 1.000000000000000000, 1.000000000000000000, 1.000000000000000000, 1.000000000000000000, 1.000000000000000000, 1.000000000000000000, 1.000000000000000000, 1.000000000000000000, 1.000000000000000000, 1.000000000000000000, 1.000000000000000000, 1.000000000000000000, 1.000000000000000000, 1.000000000000000000, 1.000000000000000000, 1.000000000000000000, 1.000000000000000000, 1.000000000000000000, 1.000000000000000000, 1.000000000000000000, 1.000000000000000000, 1.000000000000000000, 1.000000000000000000, 1.000000000000000000, 1.000000000000000000, 1.000000000000000000, 1.000000000000000000, 1.000000000000000000, 1.000000000000000000, 1.000000000000000000, 1.000000000000000000, 1.000000000000000000, 1.000000000000000000, 1.000000000000000000, 1.000000000000000000, 1.000000000000000000, 1.000000000000000000, 1.000000000000000000, 1.000000000000000000),
 ( 0.3333333333333333703, 0.3333333333333333703, 0.3333333333333333703, 0.3333333333333333703, 0.3333333333333333703, 0.3333333333333333703, 0.3333333333333333703, 0.3333333333333333703, 0.3333333333333333703, 0.3333333333333333703, 0.3333333333333333703, 0.3333333333333333703, 0.3333333333333333703, 0.3333333333333333703, 0.3333333333333333703, 0.3333333333333333703, 0.3333333333333333703, 0.3333333333333333703, 0.3333333333333333703, 0.3333333333333333703, 0.3333333333333333703, 0.3333333333333333703, 0.3333333333333333703, 0.3333333333333333703, 0.3333333333333333703, 0.3333333333333333703, 0.3333333333333333703, 0.3333333333333333703, 0.3333333333333333703, 0.3333333333333333703, 0.3333333333333333703, 0.3333333333333333703, 0.3333333333333333703, 0.3333333333333333703, 0.3333333333333333703, 0.3333333333333333703, 0.3333333333333333703, 0.3333333333333333703, 0.3333333333333333703, 0.3333333333333333703),
 ( 0.3333333333333333703, 0.3333333333333333703, 0.3333333333333333703, 0.3333333333333333703, 0.3333333333333333703, 0.3333333333333333703, 0.3333333333333333703, 0.3333333333333333703, 0.3333333333333333703, 0.3333333333333333703, 0.3333333333333333703, 0.3333333333333333703, 0.3333333333333333703, 0.3333333333333333703, 0.3333333333333333703, 0.3333333333333333703, 0.3333333333333333703, 0.3333333333333333703, 0.3333333333333333703, 0.3333333333333333703, 0.3333333333333333703, 0.3333333333333333703, 0.3333333333333333703, 0.3333333333333333703, 0.3333333333333333703, 0.3333333333333333703, 0.3333333333333333703, 0.3333333333333333703, 0.3333333333333333703, 0.3333333333333333703, 0.3333333333333333703, 0.3333333333333333703, 0.3333333333333333703, 0.3333333333333333703, 0.3333333333333333703, 0.3333333333333333703, 0.3333333333333333703, 0.3333333333333333703, 0.3333333333333333703, 0.3333333333333333703),
 ( 1.000000000000000000, 1.000000000000000000, 1.000000000000000000, 1.000000000000000000, 1.000000000000000000, 1.000000000000000000, 1.000000000000000000, 1.000000000000000000, 1.000000000000000000, 1.000000000000000000, 1.000000000000000000, 1.000000000000000000, 1.000000000000000000, 1.000000000000000000, 1.000000000000000000, 1.000000000000000000, 1.000000000000000000, 1.000000000000000000, 1.000000000000000000, 1.000000000000000000, 1.000000000000000000, 1.000000000000000000, 1.000000000000000000, 1.000000000000000000, 1.000000000000000000, 1.000000000000000000, 1.000000000000000000, 1.000000000000000000, 1.000000000000000000, 1.000000000000000000, 1.000000000000000000, 1.000000000000000000, 1.000000000000000000, 1.000000000000000000, 1.000000000000000000, 1.000000000000000000, 1.000000000000000000, 1.000000000000000000, 1.000000000000000000, 1.000000000000000000) ) ) 
 REPRESENTATION_ITEM ( '' )  SURFACE ( )  );
#20474 = DIRECTION ( 'NONE',  ( 0.000000000000000000, 1.000000000000000000, 0.000000000000000000 ) ) ;
#20475 = CARTESIAN_POINT ( 'NONE',  ( 2.916276642307554123, -11.05036367517186058, 2.119705115445599475 ) ) ;
#20476 = DIRECTION ( 'NONE',  ( 1.000000000000000000, 0.000000000000000000, -0.000000000000000000 ) ) ;
#20477 = CARTESIAN_POINT ( 'NONE',  ( 13.10372118337080849, 3.925419760224517329, 6.005889426248455010 ) ) ;
#20478 = FACE_OUTER_BOUND ( 'NONE', #10566, .T. ) ;
#20479 = DIRECTION ( 'NONE',  ( 0.000000000000000000, 0.000000000000000000, 1.000000000000000000 ) ) ;
#20480 = DIRECTION ( 'NONE',  ( -1.000000000000000000, 0.000000000000000000, 0.000000000000000000 ) ) ;
#20481 = CARTESIAN_POINT ( 'NONE',  ( 5.409691417683178294, -21.63647391050456648, 4.520995438708348857 ) ) ;
#20482 = CARTESIAN_POINT ( 'NONE',  ( -12.62499999999998401, -19.49999999999998934, 3.146526952850934755 ) ) ;
#20483 = CARTESIAN_POINT ( 'NONE',  ( -10.74655858231679595, -21.94931252712234127, 4.499999999999999112 ) ) ;
#20484 = VECTOR ( 'NONE', #9772, 1000.000000000000000 ) ;
#20485 = CARTESIAN_POINT ( 'NONE',  ( -6.722191417683176518, -19.52099543870834353, 4.586221378810406257 ) ) ;
#20486 = ORIENTED_EDGE ( 'NONE', *, *, #4892, .T. ) ;
#20487 = CARTESIAN_POINT ( 'NONE',  ( 13.07840392524817474, 3.396898225032857432, 5.244490940007585422 ) ) ;
#20488 = LINE ( 'NONE', #7712, #3307 ) ;
#20489 = ADVANCED_FACE ( 'NONE', ( #2636 ), #18446, .T. ) ;
#20490 = VERTEX_POINT ( 'NONE', #7044 ) ;
#20491 = PLANE ( 'NONE',  #14976 ) ;
#20492 = ORIENTED_EDGE ( 'NONE', *, *, #301, .F. ) ;
#20493 = CARTESIAN_POINT ( 'NONE',  ( 3.162271481458107658, -13.95306990448253437, 3.615178062515473911 ) ) ;
#20494 = ORIENTED_EDGE ( 'NONE', *, *, #2905, .T. ) ;
#20495 = LINE ( 'NONE', #15349, #11987 ) ;
#20496 = CIRCLE ( 'NONE', #11459, 10.00000000000000000 ) ;
#20497 = FACE_OUTER_BOUND ( 'NONE', #1228, .T. ) ;
#20498 = EDGE_CURVE ( 'NONE', #7526, #8019, #19917, .T. ) ;
#20499 = CARTESIAN_POINT ( 'NONE',  ( -2.282685604506861754, -11.80366834561962364, 2.120553820834011116 ) ) ;
#20500 = DIRECTION ( 'NONE',  ( 1.000000000000000000, 0.000000000000000000, -0.000000000000000000 ) ) ;
#20501 = LINE ( 'NONE', #14092, #12032 ) ;
#20502 = CARTESIAN_POINT ( 'NONE',  ( -11.00000000000000000, -24.49999999999999289, 4.000000000000000000 ) ) ;
#20503 = ADVANCED_FACE ( 'NONE', ( #13412 ), #5471, .F. ) ;
#20504 = ADVANCED_FACE ( 'NONE', ( #10277 ), #2527, .T. ) ;
#20505 = CARTESIAN_POINT ( 'NONE',  ( 3.944195004867014909, -21.42722504787766624, 5.934029185143018914 ) ) ;
#20506 = PLANE ( 'NONE',  #17213 ) ;
#20507 = CARTESIAN_POINT ( 'NONE',  ( -7.097191417683177406, -22.77556120703057729, 5.229004561291655584 ) ) ;
#20508 = ORIENTED_EDGE ( 'NONE', *, *, #11522, .T. ) ;
#20509 = CARTESIAN_POINT ( 'NONE',  ( 6.340308582316793284, -22.67418626127525982, 5.270995438708342640 ) ) ;
#20510 = LINE ( 'NONE', #8043, #2742 ) ;
#20511 = CARTESIAN_POINT ( 'NONE',  ( -12.73577686058281344, -15.40576854059989920, 6.340204579155907183 ) ) ;
#20512 = ORIENTED_EDGE ( 'NONE', *, *, #5809, .T. ) ;
#20513 = CARTESIAN_POINT ( 'NONE',  ( 8.121558582316792396, -23.74999999999999645, 3.550687472877651629 ) ) ;
#20514 = DIRECTION ( 'NONE',  ( 1.000000000000000000, 0.000000000000000000, 0.000000000000000000 ) ) ;
#20515 = ORIENTED_EDGE ( 'NONE', *, *, #19919, .T. ) ;
#20516 = LINE ( 'NONE', #10134, #19309 ) ;
#20517 =( NAMED_UNIT ( * ) SI_UNIT ( $, .STERADIAN. ) SOLID_ANGLE_UNIT ( ) );
#20518 = EDGE_LOOP ( 'NONE', ( #16398, #790, #2949, #13637 ) ) ;
#20519 = CARTESIAN_POINT ( 'NONE',  ( -11.75209451496117197, 10.00000000000000000, 0.000000000000000000 ) ) ;
#20520 = VERTEX_POINT ( 'NONE', #964 ) ;
#20521 = DIRECTION ( 'NONE',  ( -1.000000000000000000, -0.000000000000000000, -0.000000000000000000 ) ) ;
#20522 = CARTESIAN_POINT ( 'NONE',  ( 12.63943061533661982, -19.52125392549825733, 5.470334935344855154 ) ) ;
#20523 = ADVANCED_FACE ( 'NONE', ( #4207 ), #8713, .T. ) ;
#20524 = CARTESIAN_POINT ( 'NONE',  ( 16.37779268661489596, 0.000000000000000000, 1.000000000000000000 ) ) ;
#20525 = CARTESIAN_POINT ( 'NONE',  ( 0.2815691515810352374, -8.364917468222230923, 1.622643865078524428 ) ) ;
#20526 = DIRECTION ( 'NONE',  ( 1.000000000000000000, 0.000000000000000000, -0.000000000000000000 ) ) ;
#20527 = CARTESIAN_POINT ( 'NONE',  ( -13.37500000000002132, -19.50000000000273559, 4.083333333315724012 ) ) ;
#20528 = CARTESIAN_POINT ( 'NONE',  ( 10.18405858231679417, -20.79840458871652942, 2.226721677130544030 ) ) ;
#20529 = CARTESIAN_POINT ( 'NONE',  ( -13.87144757537903494, 4.070602556641903291, 6.741633940066556363 ) ) ;
#20530 = DIRECTION ( 'NONE',  ( 0.000000000000000000, 1.000000000000000000, -0.000000000000000000 ) ) ;
#20531 = CARTESIAN_POINT ( 'NONE',  ( 6.621558582316794173, -23.74999999999999645, 3.550687472877651629 ) ) ;
#20532 = EDGE_CURVE ( 'NONE', #6863, #20379, #17697, .T. ) ;
#20533 = CARTESIAN_POINT ( 'NONE',  ( 8.784691417683177406, -23.02099543870834353, 3.863526089495429972 ) ) ;
#20534 = CARTESIAN_POINT ( 'NONE',  ( -11.97219141768317563, -23.72900456129164937, 2.724438792969417378 ) ) ;
#20535 = ORIENTED_EDGE ( 'NONE', *, *, #14507, .F. ) ;
#20536 = CARTESIAN_POINT ( 'NONE',  ( 13.38269957179998038, -19.11117162410040038, 4.745921838382382241 ) ) ;
#20537 = CARTESIAN_POINT ( 'NONE',  ( -1.337453470010121714, -9.114917468222230923, 1.622643865078341463 ) ) ;
#20538 = VERTEX_POINT ( 'NONE', #7767 ) ;
#20539 = UNCERTAINTY_MEASURE_WITH_UNIT (LENGTH_MEASURE( 1.000000000000000082E-05 ), #17046, 'distance_accuracy_value', 'NONE');
#20540 = ORIENTED_EDGE ( 'NONE', *, *, #4200, .T. ) ;
#20541 = DIRECTION ( 'NONE',  ( 1.000000000000000000, 0.000000000000000000, 0.000000000000000000 ) ) ;
#20542 = CARTESIAN_POINT ( 'NONE',  ( -12.64195242771744709, -19.39390240027112000, 5.496549442168085164 ) ) ;
#20543 = EDGE_CURVE ( 'NONE', #14392, #8942, #9799, .T. ) ;
#20544 = ADVANCED_FACE ( 'NONE', ( #1179 ), #11110, .T. ) ;
#20545 = CARTESIAN_POINT ( 'NONE',  ( -1.655860418491166941, -9.114909740826840689, 2.372641880528837621 ) ) ;
#20546 = CARTESIAN_POINT ( 'NONE',  ( -13.41820805991576826, -18.06799297425606454, 5.518388032956592859 ) ) ;
#20547 = ADVANCED_FACE ( 'NONE', ( #7557 ), #7863, .T. ) ;
#20548 = CARTESIAN_POINT ( 'NONE',  ( -14.49999999999998579, -18.49999999999999645, 1.000000000000000000 ) ) ;
#20549 = DIRECTION ( 'NONE',  ( -1.000000000000000000, -0.000000000000000000, -0.000000000000000000 ) ) ;
#20550 = DIRECTION ( 'NONE',  ( -0.000000000000000000, -0.000000000000000000, -1.000000000000000000 ) ) ;
#20551 = LINE ( 'NONE', #3172, #14395 ) ;
#20552 = CARTESIAN_POINT ( 'NONE',  ( 13.15452713448031297, 5.741120291255121799, 5.290164123766007087 ) ) ;
#20553 = CARTESIAN_POINT ( 'NONE',  ( -10.65969141768317741, -22.98484643305507191, 0.9790045612916508100 ) ) ;
#20554 = CARTESIAN_POINT ( 'NONE',  ( -1.742625132518061504, -9.872369070458363538, 2.374557585393312298 ) ) ;
#20555 = ORIENTED_EDGE ( 'NONE', *, *, #9322, .F. ) ;
#20556 = CARTESIAN_POINT ( 'NONE',  ( -13.83531008031826026, 3.745659056069631898, 5.237458296715707284 ) ) ;
#20557 = CARTESIAN_POINT ( 'NONE',  ( -17.94064177244175795, 0.000000000000000000, 1.000000000000000000 ) ) ;
#20558 = CARTESIAN_POINT ( 'NONE',  ( 5.784691417683178294, -24.52099543870834708, 4.484846433055073689 ) ) ;
#20559 = CARTESIAN_POINT ( 'NONE',  ( -5.690941417683177406, -22.74294823697955081, 4.171265325393542334 ) ) ;
#20560 = VERTEX_POINT ( 'NONE', #18858 ) ;
#20561 = CARTESIAN_POINT ( 'NONE',  ( 13.87470602645761986, 4.985154336109792972, 4.791666666666685614 ) ) ;
#20562 = DIRECTION ( 'NONE',  ( 1.000000000000000000, 0.000000000000000000, -0.000000000000000000 ) ) ;
#20563 = FACE_OUTER_BOUND ( 'NONE', #20249, .T. ) ;
#20564 = EDGE_LOOP ( 'NONE', ( #3082, #14645, #18987, #832 ) ) ;
#20565 = ORIENTED_EDGE ( 'NONE', *, *, #4912, .F. ) ;
#20566 = CARTESIAN_POINT ( 'NONE',  ( 0.000000000000000000, 4.999999999999999112, 0.000000000000000000 ) ) ;
#20567 = VECTOR ( 'NONE', #10841, 1000.000000000000000 ) ;
#20568 = CARTESIAN_POINT ( 'NONE',  ( -13.97248077590530180, -0.1818351014256275322, 0.8937704884164922037 ) ) ;
#20569 = ORIENTED_EDGE ( 'NONE', *, *, #13895, .F. ) ;
#20570 = CARTESIAN_POINT ( 'NONE',  ( -26.94203811574920593, 0.000000000000000000, 1.000000000000000000 ) ) ;
#20571 = CARTESIAN_POINT ( 'NONE',  ( 17.12779268661489596, 16.00000000000000000, 1.000000000000000000 ) ) ;
#20572 = CARTESIAN_POINT ( 'NONE',  ( -10.43924542913431175, 10.00000000000000000, 0.000000000000000000 ) ) ;
#20573 = CARTESIAN_POINT ( 'NONE',  ( 3.187906586576829682, -9.105473976199601083, 1.812833570429532859 ) ) ;
#20574 = DIRECTION ( 'NONE',  ( -0.000000000000000000, -0.000000000000000000, -1.000000000000000000 ) ) ;
#20575 = CARTESIAN_POINT ( 'NONE',  ( -1.561130159782011306, 0.000000000000000000, 1.000000000000000000 ) ) ;
#20576 = CARTESIAN_POINT ( 'NONE',  ( 30.00000000000000000, 10.00000000000000000, 1.000000000000000000 ) ) ;
#20577 = DIRECTION ( 'NONE',  ( -1.000000000000000000, 0.000000000000000000, 0.000000000000000000 ) ) ;
#20578 = DIRECTION ( 'NONE',  ( -0.000000000000000000, 0.000000000000000000, -1.000000000000000000 ) ) ;
#20579 = CARTESIAN_POINT ( 'NONE',  ( 4.284691417683177406, -23.02099543870834353, 3.863526089495429972 ) ) ;
#20580 = CARTESIAN_POINT ( 'NONE',  ( -13.12529397354238192, 5.014845663890295846, 4.791666666666685614 ) ) ;
#20581 = CARTESIAN_POINT ( 'NONE',  ( -12.43405858231679595, -22.67126532539354855, 4.242948236979545484 ) ) ;
#20582 = ADVANCED_FACE ( 'NONE', ( #6096 ), #12660, .T. ) ;
#20583 = CARTESIAN_POINT ( 'NONE',  ( -4.472191417683178294, -24.47900456129165292, 2.413778621189595963 ) ) ;
#20584 = VERTEX_POINT ( 'NONE', #17267 ) ;
#20585 = CARTESIAN_POINT ( 'NONE',  ( 13.09560264576187905, 4.265433610975056133, 4.166666666666765551 ) ) ;
#20586 = DIRECTION ( 'NONE',  ( 0.000000000000000000, 0.000000000000000000, 1.000000000000000000 ) ) ;
#20587 = ORIENTED_EDGE ( 'NONE', *, *, #10257, .T. ) ;
#20588 = PLANE ( 'NONE',  #10641 ) ;
#20589 = ORIENTED_EDGE ( 'NONE', *, *, #9355, .T. ) ;
#20590 = CARTESIAN_POINT ( 'NONE',  ( 2.583953725994688533, -9.847075946378776479, 2.560676788604062004 ) ) ;
#20591 = ADVANCED_FACE ( 'NONE', ( #2946 ), #1582, .T. ) ;
#20592 = ORIENTED_EDGE ( 'NONE', *, *, #4302, .F. ) ;
#20593 = CARTESIAN_POINT ( 'NONE',  ( 7.753441417683176518, -21.94931252712233061, 1.749999999999998446 ) ) ;
#20594 = PLANE ( 'NONE',  #19004 ) ;
#20595 = CARTESIAN_POINT ( 'NONE',  ( -0.2815691515810352930, -9.114917468222230923, 1.622643865078524206 ) ) ;
#20596 = FACE_OUTER_BOUND ( 'NONE', #7713, .T. ) ;
#20597 = CARTESIAN_POINT ( 'NONE',  ( 0.3749999999999968914, 9.000000000000000000, 0.000000000000000000 ) ) ;
#20598 = LINE ( 'NONE', #8810, #11300 ) ;
#20599 = CARTESIAN_POINT ( 'NONE',  ( 7.003441417683177406, -22.05068747287766229, 6.000000000000001776 ) ) ;
#20600 = DIRECTION ( 'NONE',  ( 0.000000000000000000, 0.000000000000000000, 1.000000000000000000 ) ) ;
#20601 = CARTESIAN_POINT ( 'NONE',  ( -10.00344141768317563, -22.05068747287765873, 5.250000000000000888 ) ) ;
#20602 = ORIENTED_EDGE ( 'NONE', *, *, #11091, .F. ) ;
#20603 = CARTESIAN_POINT ( 'NONE',  ( 8.121558582316792396, -23.74999999999999645, 3.550687472877651629 ) ) ;
#20604 = LINE ( 'NONE', #9404, #12414 ) ;
#20605 = CARTESIAN_POINT ( 'NONE',  ( -13.90439735423812273, 5.734566389025032684, 4.833333333333343695 ) ) ;
#20606 = ORIENTED_EDGE ( 'NONE', *, *, #10082, .T. ) ;
#20607 = AXIS2_PLACEMENT_3D ( 'NONE', #13467, #4239, #9057 ) ;
#20608 = EDGE_CURVE ( 'NONE', #2127, #5816, #3332, .T. ) ;
#20609 = CARTESIAN_POINT ( 'NONE',  ( 7.090308582316794173, -21.32581373872472597, 1.729004561291657582 ) ) ;
#20610 = CARTESIAN_POINT ( 'NONE',  ( -13.50000000000000178, 5.000000000000047962, 2.000000000000000000 ) ) ;
#20611 = ORIENTED_EDGE ( 'NONE', *, *, #20656, .F. ) ;
#20612 = DIRECTION ( 'NONE',  ( -0.1351665943404306014, -0.9596796555888912339, 0.2464649070825229438 ) ) ;
#20613 = ORIENTED_EDGE ( 'NONE', *, *, #17937, .T. ) ;
#20614 = DIRECTION ( 'NONE',  ( 1.000000000000000000, -0.000000000000000000, 0.000000000000000000 ) ) ;
#20615 = EDGE_CURVE ( 'NONE', #14392, #2288, #18378, .T. ) ;
#20616 = ADVANCED_FACE ( 'NONE', ( #19173 ), #20438, .T. ) ;
#20617 = ORIENTED_EDGE ( 'NONE', *, *, #1, .F. ) ;
#20618 = CARTESIAN_POINT ( 'NONE',  ( -8.027808582316792396, -23.72900456129165647, 4.275561207030568411 ) ) ;
#20619 = LINE ( 'NONE', #11394, #18970 ) ;
#20620 = CARTESIAN_POINT ( 'NONE',  ( 0.000000000000000000, 4.999999999999999112, 0.000000000000000000 ) ) ;
#20621 = CARTESIAN_POINT ( 'NONE',  ( 1.337453470010121714, -9.864917468222230923, 1.622643865078341907 ) ) ;
#20622 = LINE ( 'NONE', #1473, #6390 ) ;
#20623 = CARTESIAN_POINT ( 'NONE',  ( -13.84090061271218985, 4.027980941966571748, 5.240332426532912535 ) ) ;
#20624 = CARTESIAN_POINT ( 'NONE',  ( 4.687312169500632564, -21.51559725698341197, 5.182386163300427562 ) ) ;
#20625 = CARTESIAN_POINT ( 'NONE',  ( -12.62527129584495000, -20.98629955982801576, 4.726243163759704657 ) ) ;
#20626 = DIRECTION ( 'NONE',  ( -0.000000000000000000, 0.000000000000000000, 1.000000000000000000 ) ) ;
#20627 = CARTESIAN_POINT ( 'NONE',  ( 5.402808582316794173, -22.77556120703056308, 1.770995438708339975 ) ) ;
#20628 = EDGE_CURVE ( 'NONE', #17249, #16180, #8078, .T. ) ;
#20629 = CARTESIAN_POINT ( 'NONE',  ( 8.597191417683177406, -22.46490103525075810, 4.479004561291653808 ) ) ;
#20630 = CARTESIAN_POINT ( 'NONE',  ( -11.78469141768317563, -23.77099543870834353, 4.174186261275251830 ) ) ;
#20631 = VERTEX_POINT ( 'NONE', #14756 ) ;
#20632 = CARTESIAN_POINT ( 'NONE',  ( 13.37939227869017600, -19.27818992614120575, 4.741950614318236390 ) ) ;
#20633 = VECTOR ( 'NONE', #7867, 1000.000000000000000 ) ;
#20634 = CARTESIAN_POINT ( 'NONE',  ( -2.012076196476103362, -9.160103213191565175, 1.634248467062433541 ) ) ;
#20635 = VERTEX_POINT ( 'NONE', #3776 ) ;
#20636 = ORIENTED_EDGE ( 'NONE', *, *, #19634, .F. ) ;
#20637 = DIRECTION ( 'NONE',  ( 0.000000000000000000, 0.9659258262890672020, -0.2588190451025246808 ) ) ;
#20638 = DIRECTION ( 'NONE',  ( 0.000000000000000000, -0.000000000000000000, 1.000000000000000000 ) ) ;
#20639 = CARTESIAN_POINT ( 'NONE',  ( -3.996922828336520794, -14.62728872172488437, 3.980945906412841850 ) ) ;
#20640 = CARTESIAN_POINT ( 'NONE',  ( 1.337453470010121714, -9.114917468222230923, 2.372643865078341019 ) ) ;
#20641 = EDGE_CURVE ( 'NONE', #15727, #1770, #13016, .T. ) ;
#20642 = CARTESIAN_POINT ( 'NONE',  ( 0.000000000000000000, 9.000000000000001776, 1.000000000000000000 ) ) ;
#20643 = CARTESIAN_POINT ( 'NONE',  ( -12.65650603190776025, -18.65894538865861563, 5.520212342915047365 ) ) ;
#20644 = DIRECTION ( 'NONE',  ( 0.000000000000000000, -1.000000000000000000, 0.000000000000000000 ) ) ;
#20645 = CARTESIAN_POINT ( 'NONE',  ( 13.15498530132288479, 5.764257716805535559, 4.916666666666649199 ) ) ;
#20646 = CARTESIAN_POINT ( 'NONE',  ( -10.28469141768317741, -24.52099543870834708, 4.484846433055073689 ) ) ;
#20647 = CARTESIAN_POINT ( 'NONE',  ( -2.011668220304084542, -11.03559989230542193, 2.673298498313999794 ) ) ;
#20648 = ORIENTED_EDGE ( 'NONE', *, *, #18360, .T. ) ;
#20649 = CARTESIAN_POINT ( 'NONE',  ( -13.37499999999998579, -20.24999999999999289, 3.666666666666653640 ) ) ;
#20650 = DIRECTION ( 'NONE',  ( 1.000000000000000000, 0.000000000000000000, 0.000000000000000000 ) ) ;
#20651 = AXIS2_PLACEMENT_3D ( 'NONE', #735, #2715, #3964 ) ;
#20652 = EDGE_CURVE ( 'NONE', #14572, #6961, #4927, .T. ) ;
#20653 = CARTESIAN_POINT ( 'NONE',  ( 7.003441417683177406, -22.05068747287766229, 6.000000000000001776 ) ) ;
#20654 = CARTESIAN_POINT ( 'NONE',  ( -7.097191417683176518, -22.46490103525075810, 4.479004561291653808 ) ) ;
#20655 = EDGE_LOOP ( 'NONE', ( #2606, #7304, #9176, #18288 ) ) ;
#20656 = EDGE_CURVE ( 'NONE', #13542, #10698, #12014, .T. ) ;
#20657 = CARTESIAN_POINT ( 'NONE',  ( 13.37499999999998401, -20.99999999999998934, 2.439580858552613751 ) ) ;
#20658 = CARTESIAN_POINT ( 'NONE',  ( 12.62499999999998579, -20.24999999999999289, 3.666666666666653640 ) ) ;
#20659 = CARTESIAN_POINT ( 'NONE',  ( 0.000000000000000000, -9.114917468222230923, 1.997643865078340797 ) ) ;
#20660 = ORIENTED_EDGE ( 'NONE', *, *, #14932, .F. ) ;
#20661 = VERTEX_POINT ( 'NONE', #14648 ) ;
#20662 = PLANE ( 'NONE',  #8439 ) ;
#20663 = LINE ( 'NONE', #14366, #3567 ) ;
#20664 = VECTOR ( 'NONE', #593, 1000.000000000000000 ) ;
#20665 = VERTEX_POINT ( 'NONE', #1694 ) ;
#20666 = DIRECTION ( 'NONE',  ( 0.000000000000000000, 1.000000000000000000, -0.000000000000000000 ) ) ;
#20667 = LINE ( 'NONE', #11521, #14686 ) ;
#20668 = CARTESIAN_POINT ( 'NONE',  ( 7.499999999999999112, -19.49999999999999645, 5.000000000000000000 ) ) ;
#20669 = CARTESIAN_POINT ( 'NONE',  ( 3.232228556578340850, -13.29361487011126464, 2.695816835751057461 ) ) ;
#20670 = CARTESIAN_POINT ( 'NONE',  ( -1.561130159782011306, 0.000000000000000000, 1.000000000000000000 ) ) ;
#20671 = DIRECTION ( 'NONE',  ( -0.000000000000000000, 1.000000000000000000, -1.304178812473495102E-15 ) ) ;
#20672 = LINE ( 'NONE', #9569, #17700 ) ;
#20673 = CARTESIAN_POINT ( 'NONE',  ( 5.000000000000000000, -7.500000000000000000, 3.160254037844365094 ) ) ;
#20674 = PLANE ( 'NONE',  #9387 ) ;
#20675 = CARTESIAN_POINT ( 'NONE',  ( -13.19432713877993812, -20.58564808021783321, 3.473490178816806662 ) ) ;
#20676 = VECTOR ( 'NONE', #19823, 1000.000000000000114 ) ;
#20677 = CARTESIAN_POINT ( 'NONE',  ( 4.003441417683175629, -22.05068747287766229, 4.499999999999999112 ) ) ;
#20678 = CARTESIAN_POINT ( 'NONE',  ( -12.83635126708105823, -9.576761012430582198, 5.715524842913705328 ) ) ;
#20679 = CARTESIAN_POINT ( 'NONE',  ( -12.43405858231679417, -23.20159541128345992, 4.773278322869455970 ) ) ;
#20680 = EDGE_CURVE ( 'NONE', #15361, #3979, #16126, .T. ) ;
#20681 = CARTESIAN_POINT ( 'NONE',  ( -11.12844141768317741, -20.24999999999999289, 3.550687472877664952 ) ) ;
#20682 = AXIS2_PLACEMENT_3D ( 'NONE', #14992, #370, #3812 ) ;
#20683 = ORIENTED_EDGE ( 'NONE', *, *, #10118, .F. ) ;
#20684 = EDGE_CURVE ( 'NONE', #5093, #965, #11412, .T. ) ;
#20685 = CARTESIAN_POINT ( 'NONE',  ( 13.08919463935856697, 3.941829287606363863, 5.256209690007596080 ) ) ;
#20686 = DIRECTION ( 'NONE',  ( -0.4999999999999949485, 0.8660254037844415942, 0.000000000000000000 ) ) ;
#20687 = ORIENTED_EDGE ( 'NONE', *, *, #16821, .F. ) ;
#20688 = LINE ( 'NONE', #11161, #5636 ) ;
#20689 = VERTEX_POINT ( 'NONE', #3669 ) ;
#20690 = PLANE ( 'NONE',  #14771 ) ;
#20691 = VECTOR ( 'NONE', #12423, 1000.000000000000000 ) ;
#20692 = VECTOR ( 'NONE', #2537, 1000.000000000000000 ) ;
#20693 = ORIENTED_EDGE ( 'NONE', *, *, #8729, .T. ) ;
#20694 = CARTESIAN_POINT ( 'NONE',  ( 10.47219141768317741, -23.72900456129164937, 2.724438792969417378 ) ) ;
#20695 = ADVANCED_FACE ( 'NONE', ( #5139 ), #19678, .T. ) ;
#20696 = CARTESIAN_POINT ( 'NONE',  ( -2.061130159782011972, 4.999999999999999112, 1.000000000000000000 ) ) ;
#20697 = VECTOR ( 'NONE', #9100, 1000.000000000000000 ) ;
#20698 = CARTESIAN_POINT ( 'NONE',  ( -3.162271481458107658, -13.95306990448253437, 3.615178062515473911 ) ) ;
#20699 = DIRECTION ( 'NONE',  ( 0.000000000000000000, 1.000000000000000000, -0.000000000000000000 ) ) ;
#20700 = CARTESIAN_POINT ( 'NONE',  ( -10.46530858231679417, -20.22900456129164937, 4.174186261275266929 ) ) ;
#20701 = VECTOR ( 'NONE', #16995, 1000.000000000000000 ) ;
#20702 = CARTESIAN_POINT ( 'NONE',  ( 8.784691417683177406, -24.52099543870834708, 4.484846433055073689 ) ) ;
#20703 = FILL_AREA_STYLE_COLOUR ( '', #4854 ) ;
#20704 = CARTESIAN_POINT ( 'NONE',  ( -9.815941417683177406, -20.79840458871654363, 4.773278322869464851 ) ) ;
#20705 = VERTEX_POINT ( 'NONE', #3464 ) ;
#20706 = CARTESIAN_POINT ( 'NONE',  ( 7.840308582316794173, -22.67418626127525982, 5.270995438708342640 ) ) ;
#20707 = VECTOR ( 'NONE', #1756, 1000.000000000000000 ) ;
#20708 = CARTESIAN_POINT ( 'NONE',  ( 0.000000000000000000, 9.000000000000001776, 1.000000000000000000 ) ) ;
#20709 = CARTESIAN_POINT ( 'NONE',  ( -13.90439735423465351, 5.734566389025032684, 3.333333333332063386 ) ) ;
#20710 = VECTOR ( 'NONE', #12805, 1000.000000000000000 ) ;
#20711 = CARTESIAN_POINT ( 'NONE',  ( 5.777808582316794173, -20.27099543870833642, 2.724438792969431589 ) ) ;
#20712 = LINE ( 'NONE', #3331, #18689 ) ;
#20713 = VECTOR ( 'NONE', #3800, 1000.000000000000000 ) ;
#20714 = VERTEX_POINT ( 'NONE', #11305 ) ;
#20715 = DIRECTION ( 'NONE',  ( 0.000000000000000000, -0.000000000000000000, 1.000000000000000000 ) ) ;
#20716 =( NAMED_UNIT ( * ) PLANE_ANGLE_UNIT ( ) SI_UNIT ( $, .RADIAN. ) );
#20717 = EDGE_LOOP ( 'NONE', ( #4452, #6608, #14516, #15139 ) ) ;
#20718 = CIRCLE ( 'NONE', #7688, 10.00000000000000000 ) ;
#20719 = CARTESIAN_POINT ( 'NONE',  ( 0.000000000000000000, -9.114917468222230923, 1.622643865078341019 ) ) ;
#20720 = NEXT_ASSEMBLY_USAGE_OCCURRENCE ( 'NAUO1', ' ', ' ', #9828, #15961, $ ) ;
#20721 = NEXT_ASSEMBLY_USAGE_OCCURRENCE ( 'NAUO2', ' ', ' ', #9828, #20327, $ ) ;
#20722 = NEXT_ASSEMBLY_USAGE_OCCURRENCE ( 'NAUO3', ' ', ' ', #9828, #19177, $ ) ;
#20723 = NEXT_ASSEMBLY_USAGE_OCCURRENCE ( 'NAUO4', ' ', ' ', #9828, #13790, $ ) ;
#20724 = NEXT_ASSEMBLY_USAGE_OCCURRENCE ( 'NAUO5', ' ', ' ', #9828, #12257, $ ) ;
ENDSEC;
END-ISO-10303-21;
